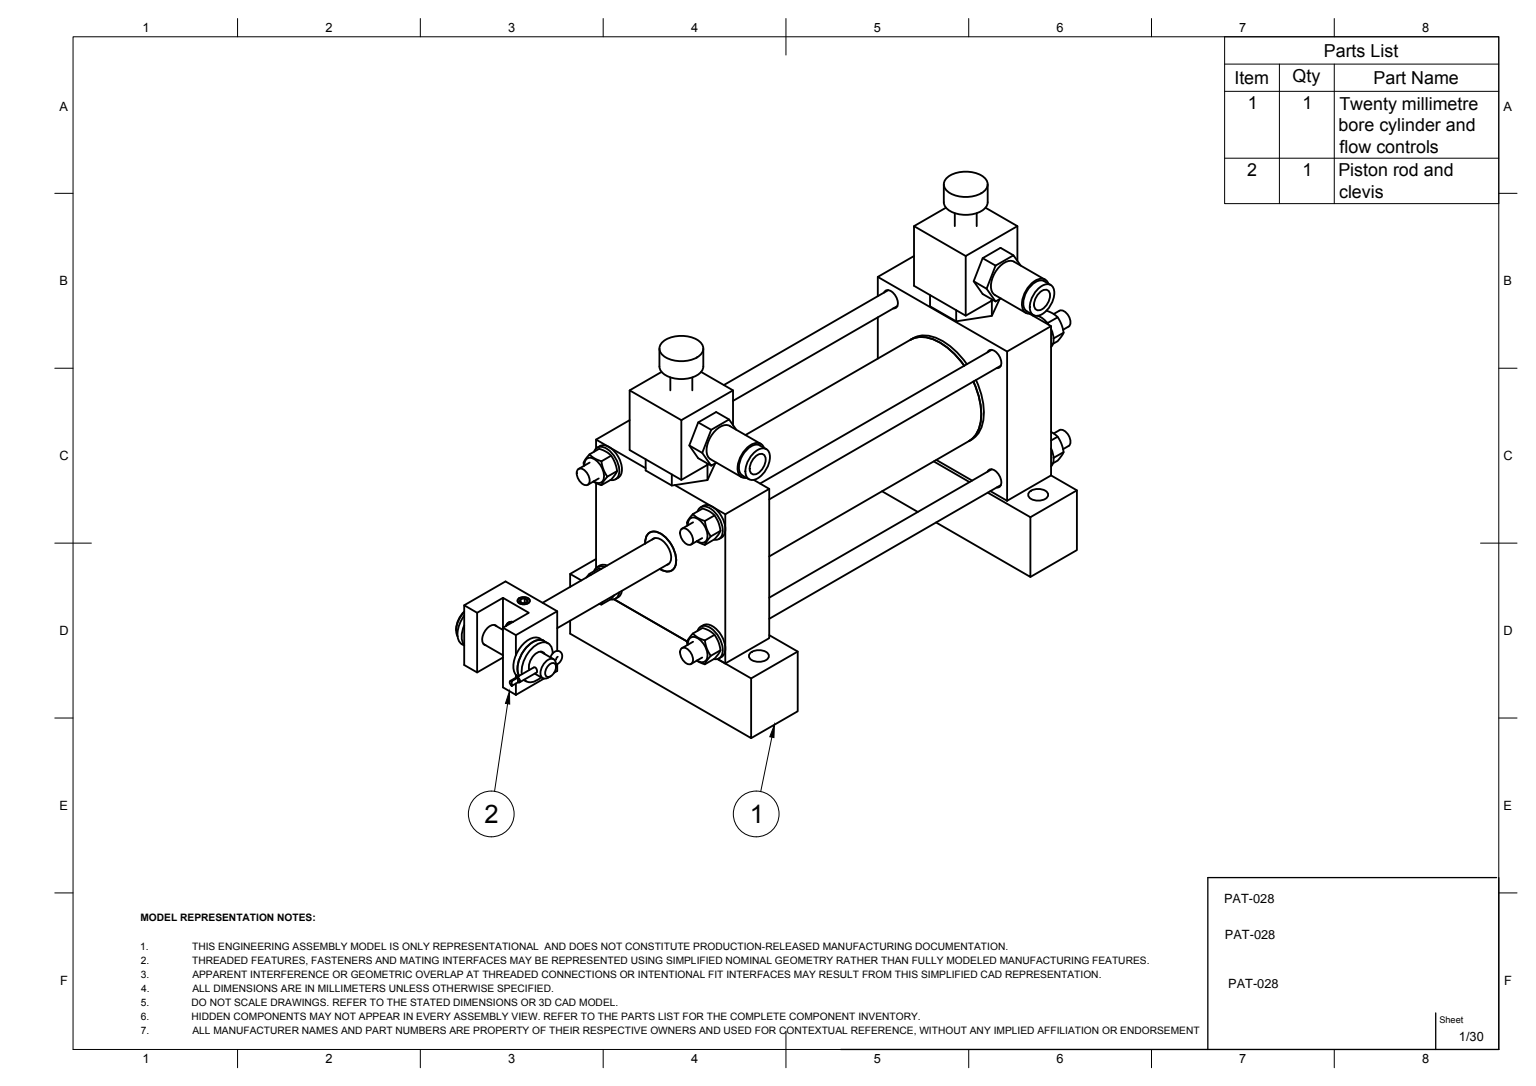
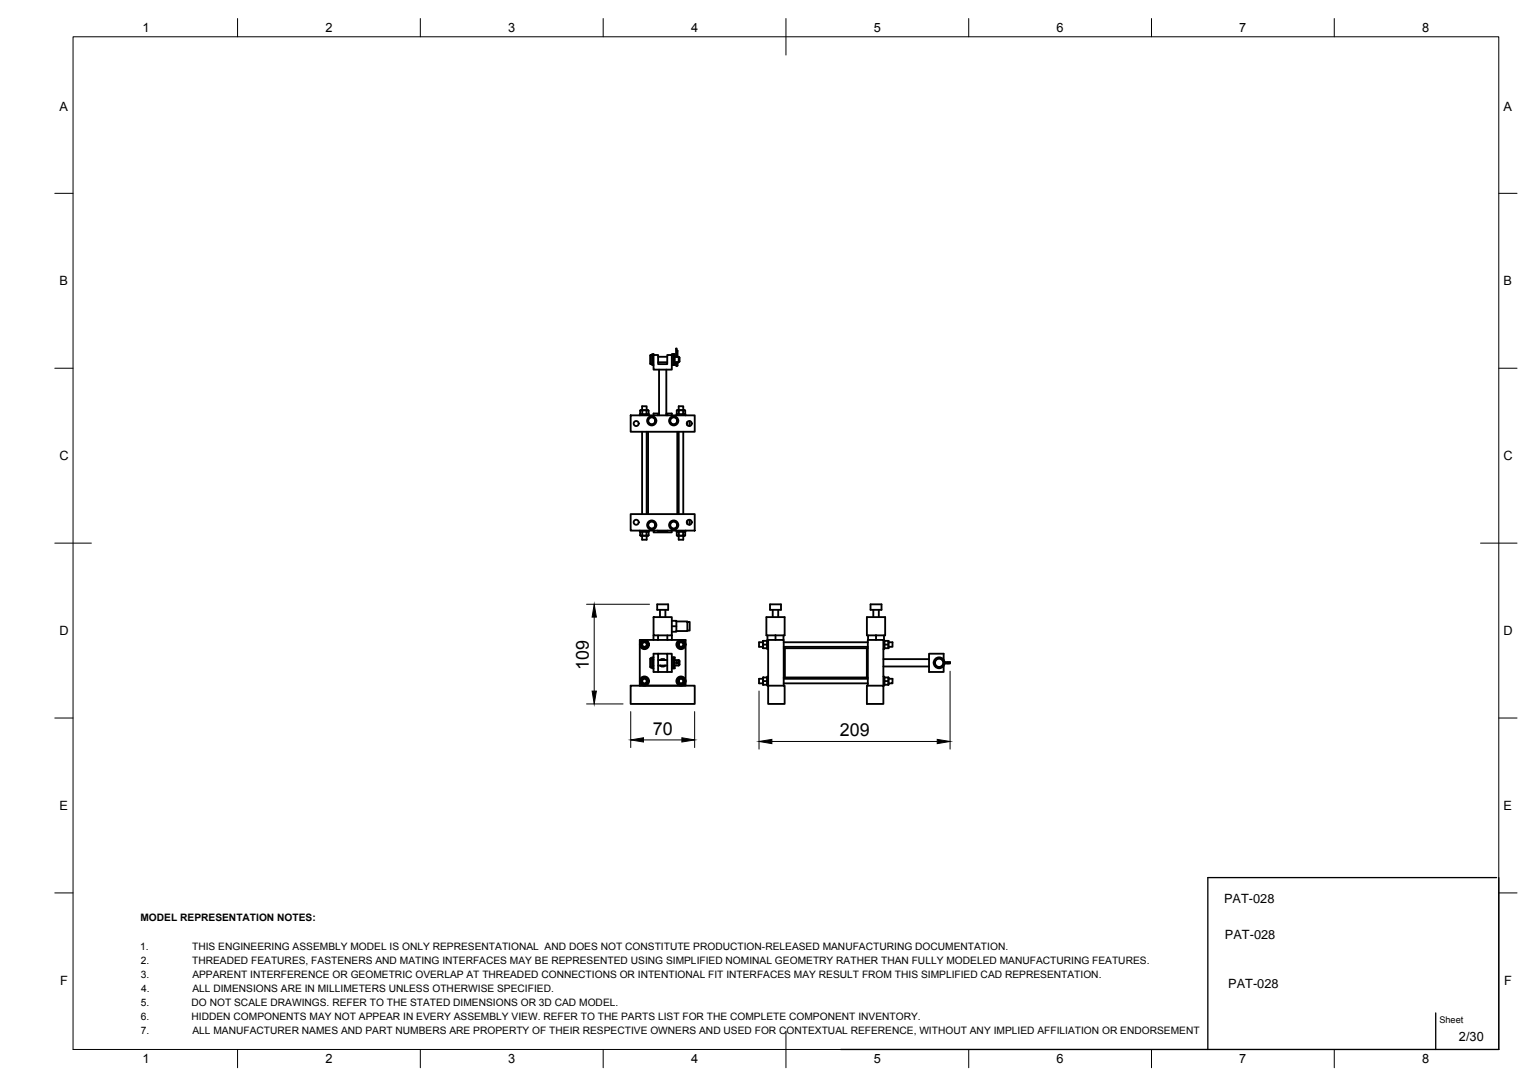
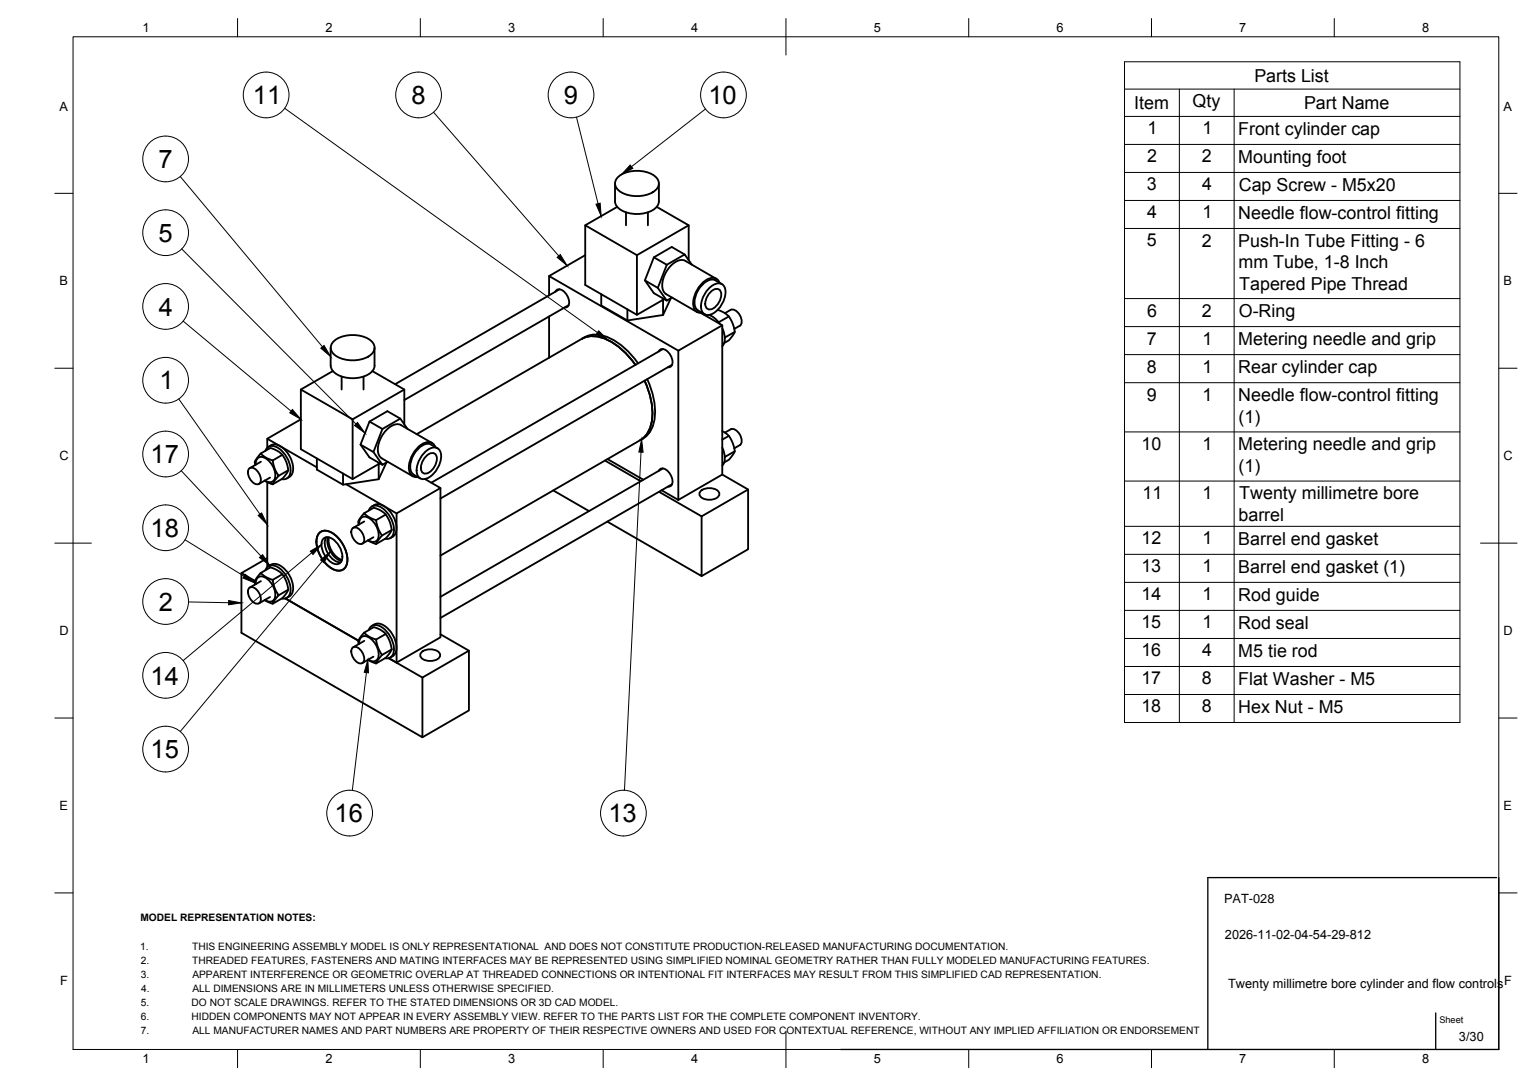
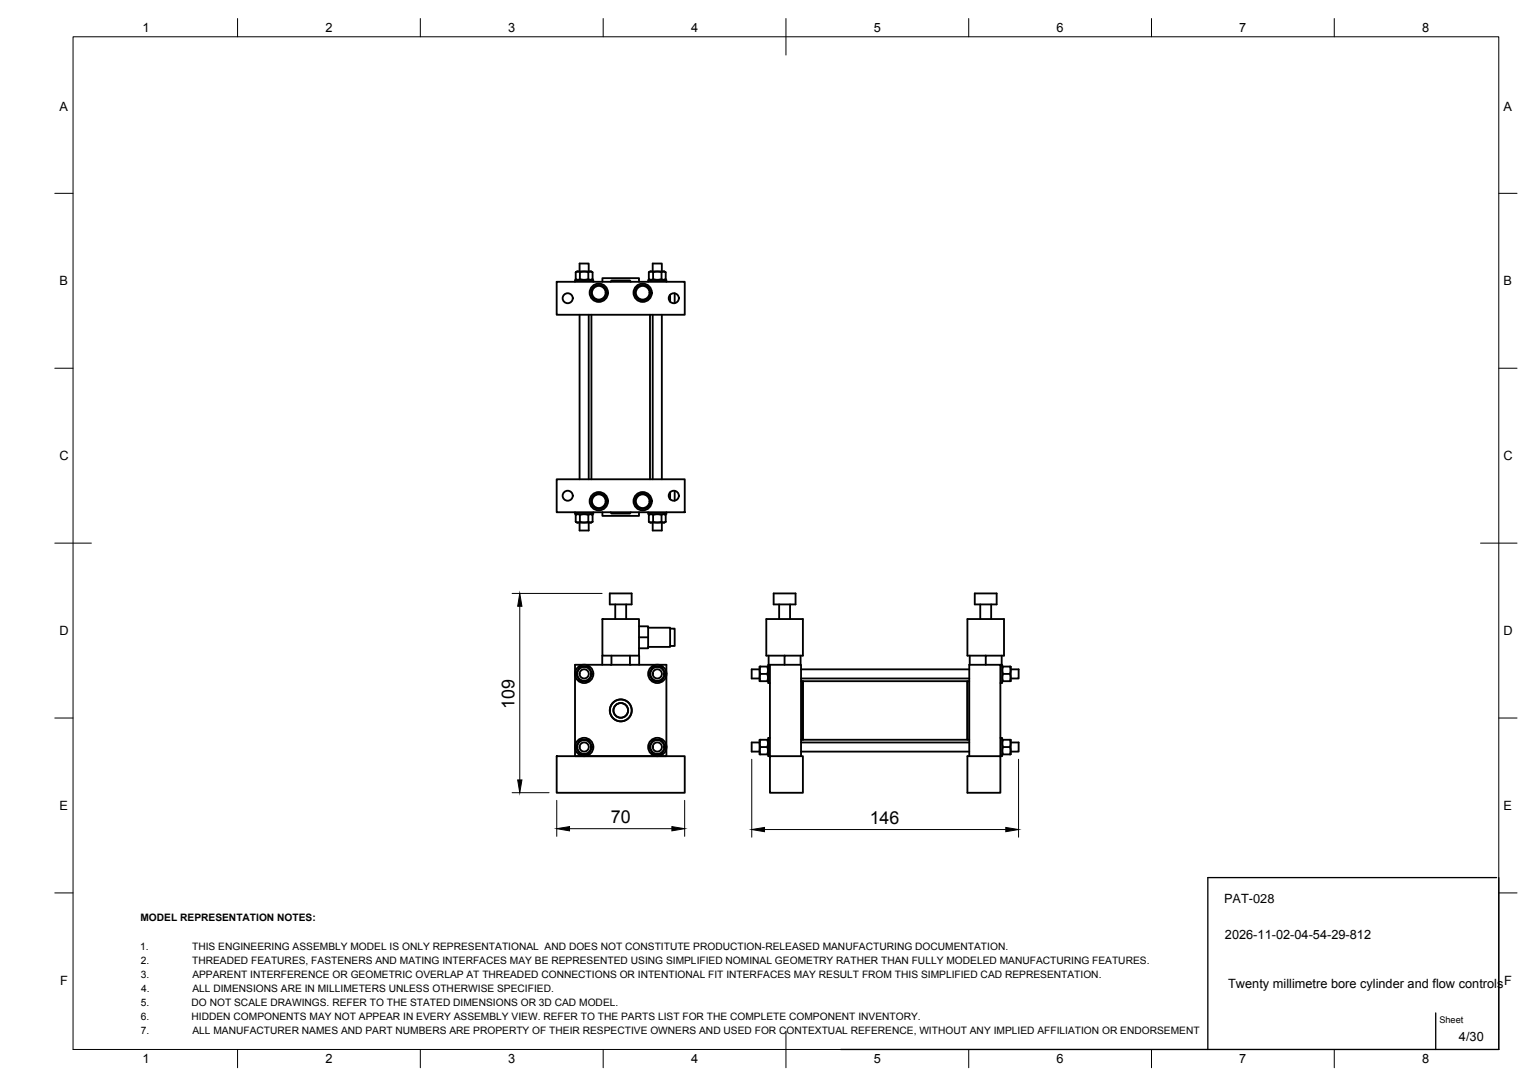
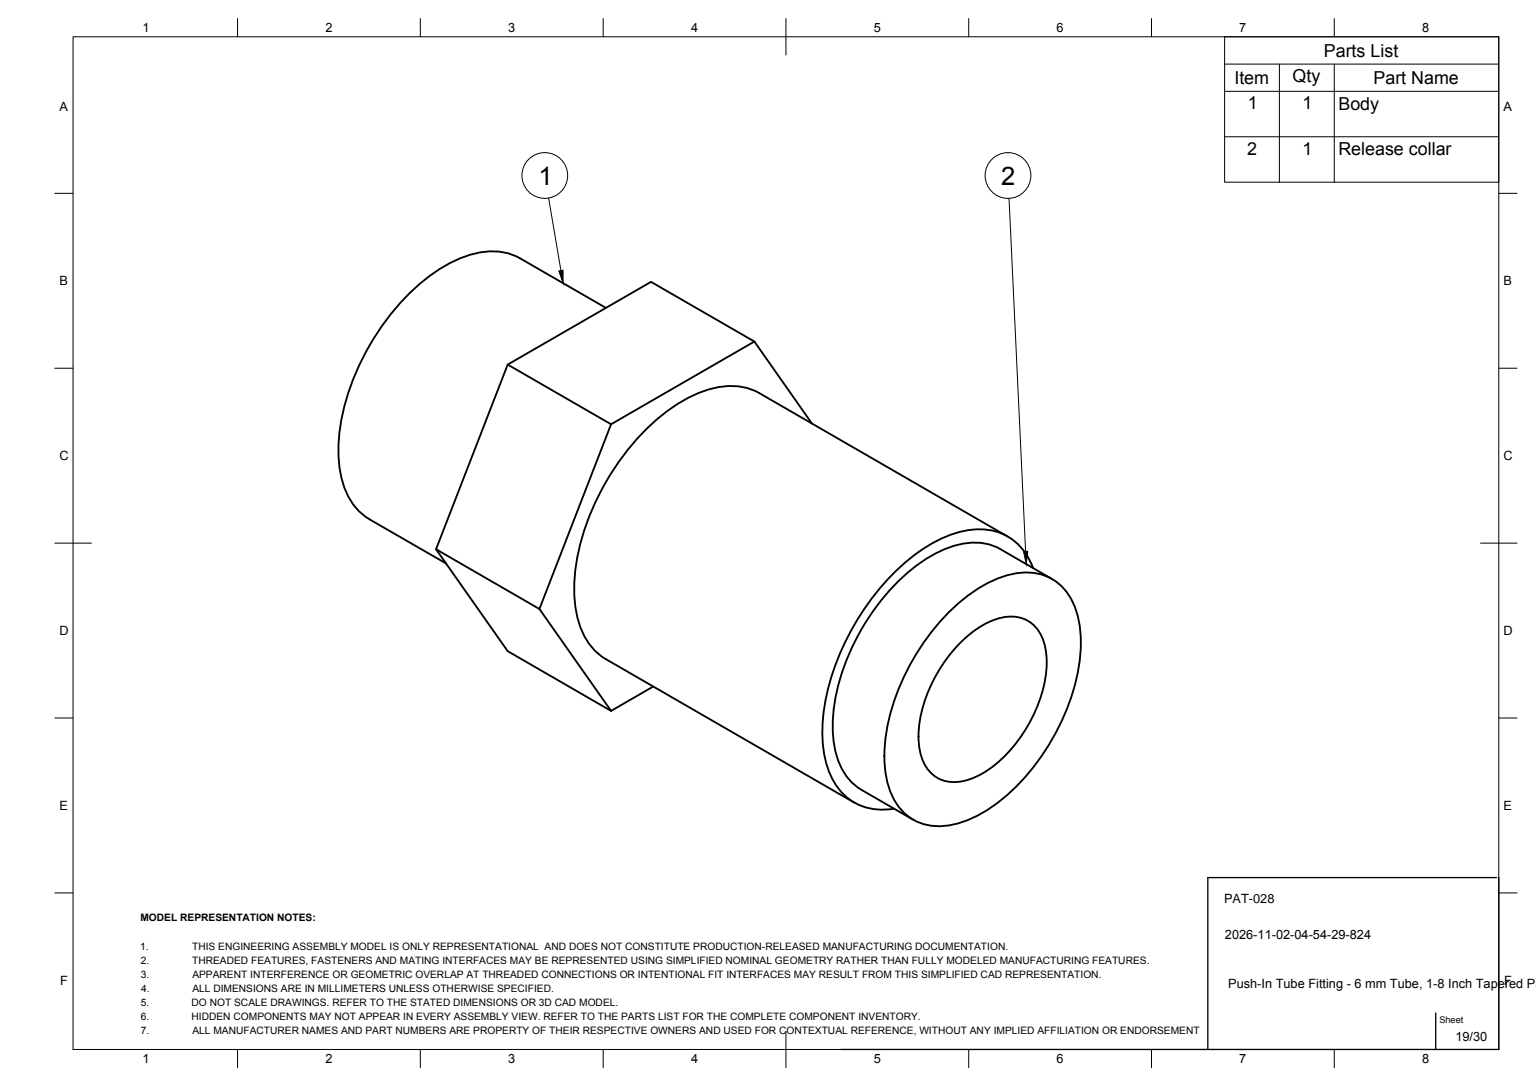
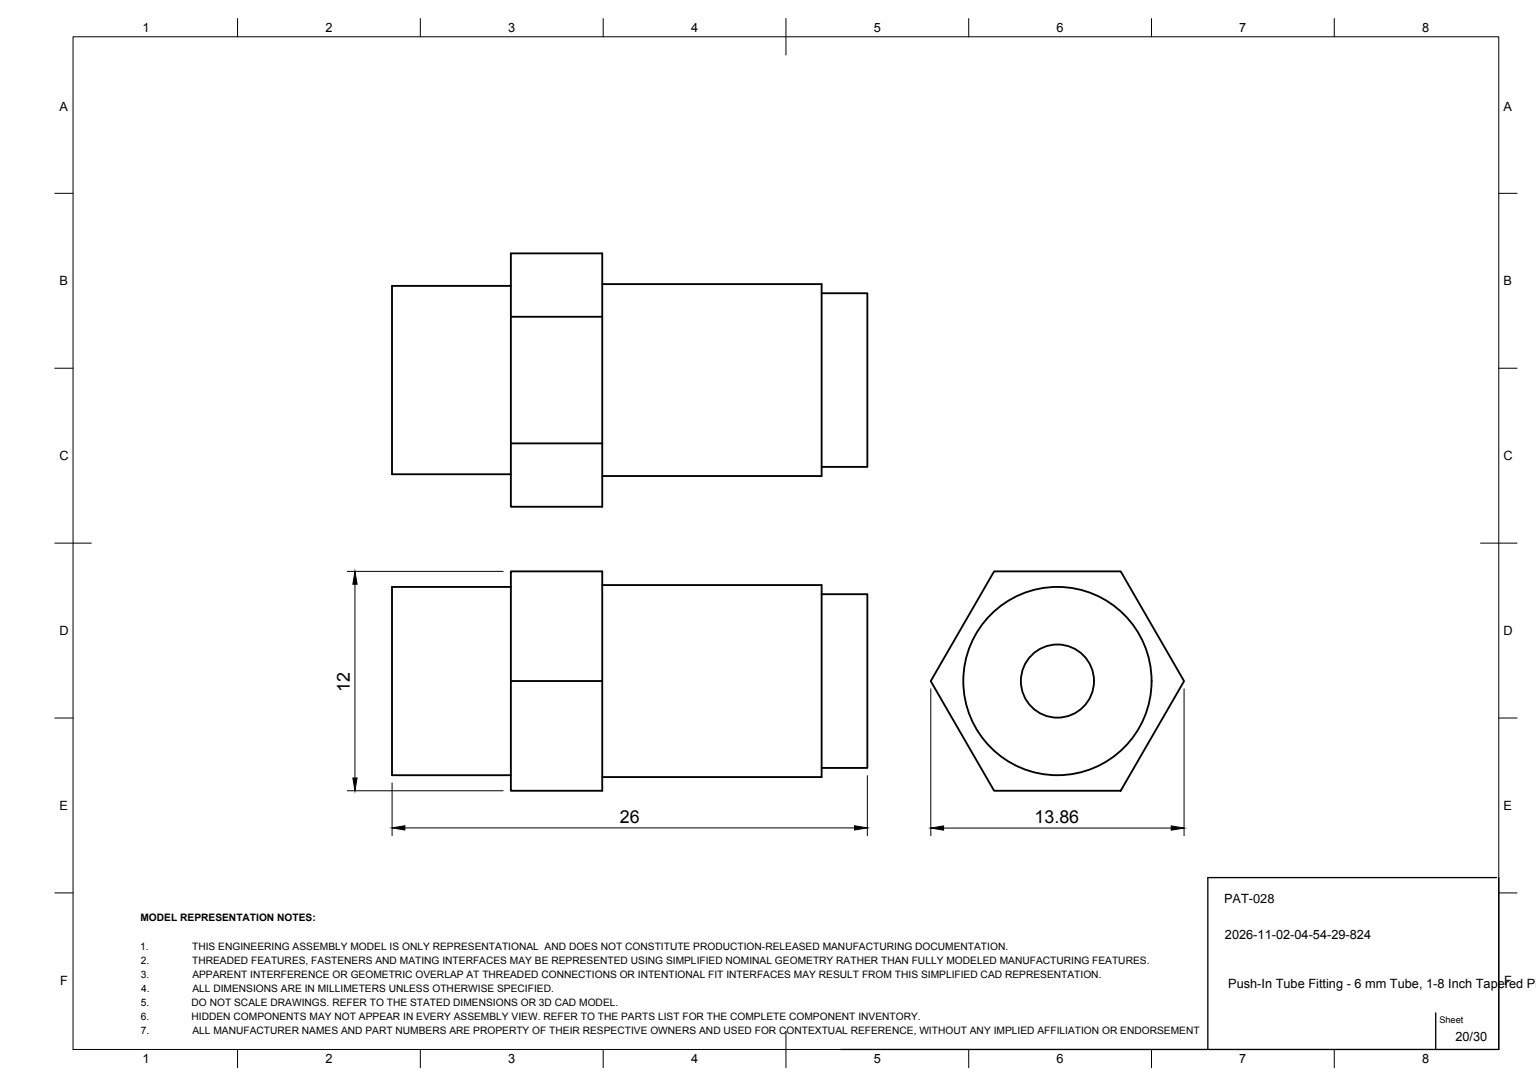
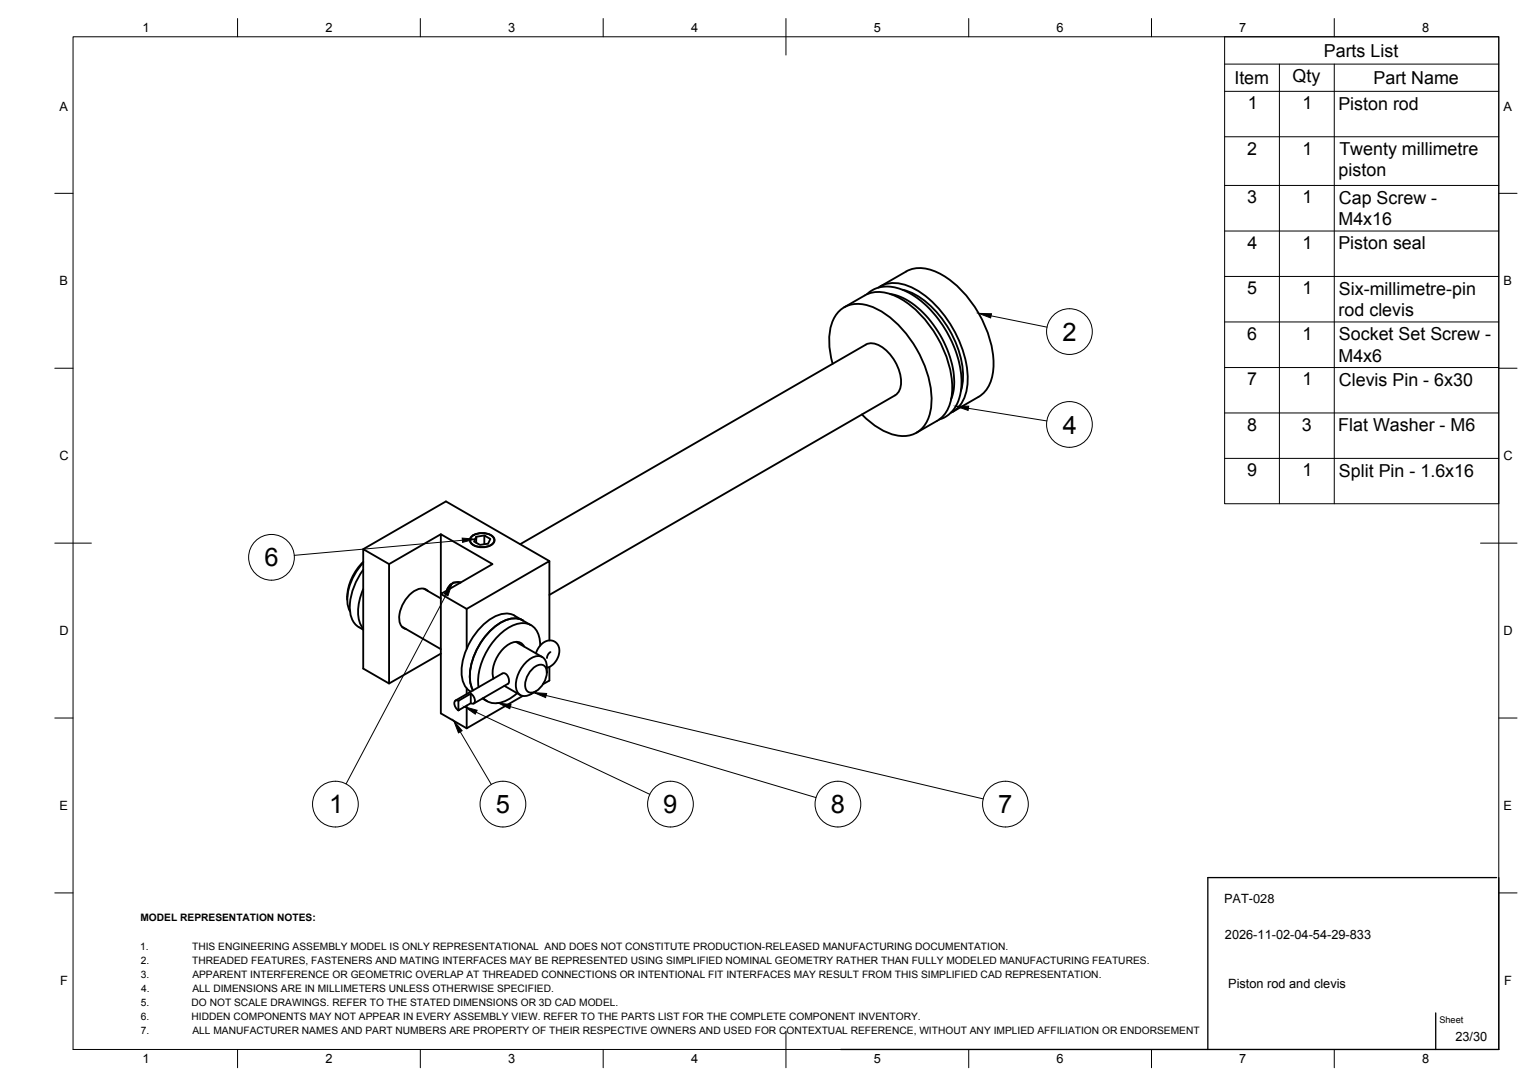
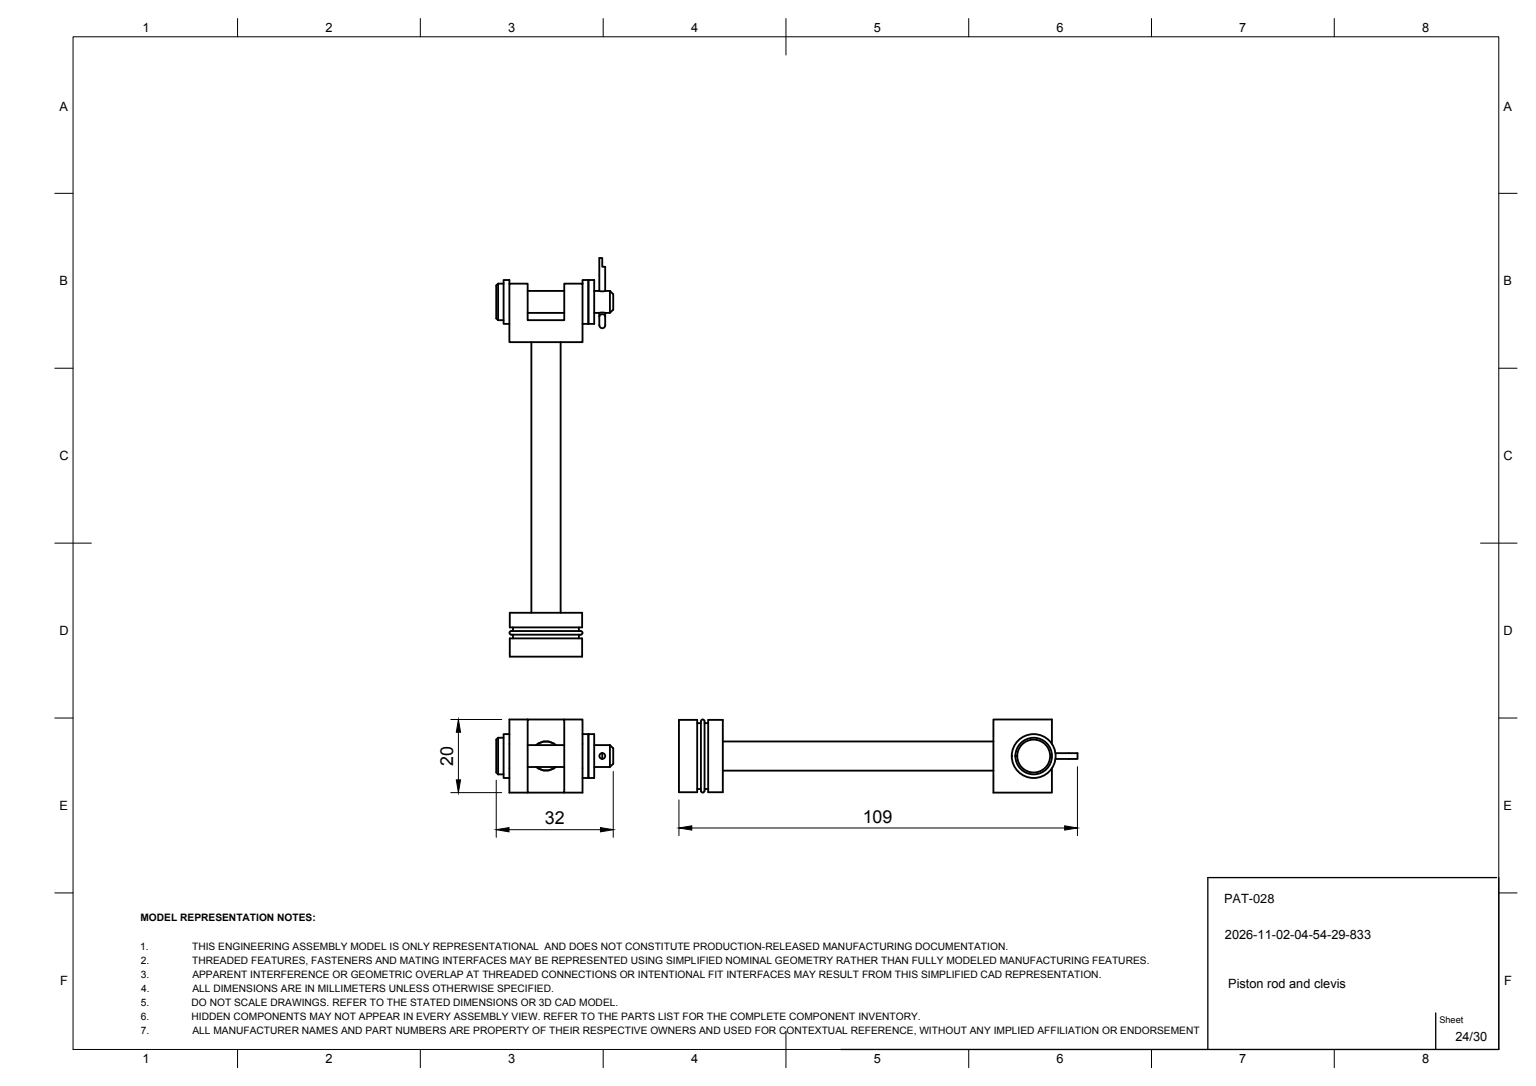
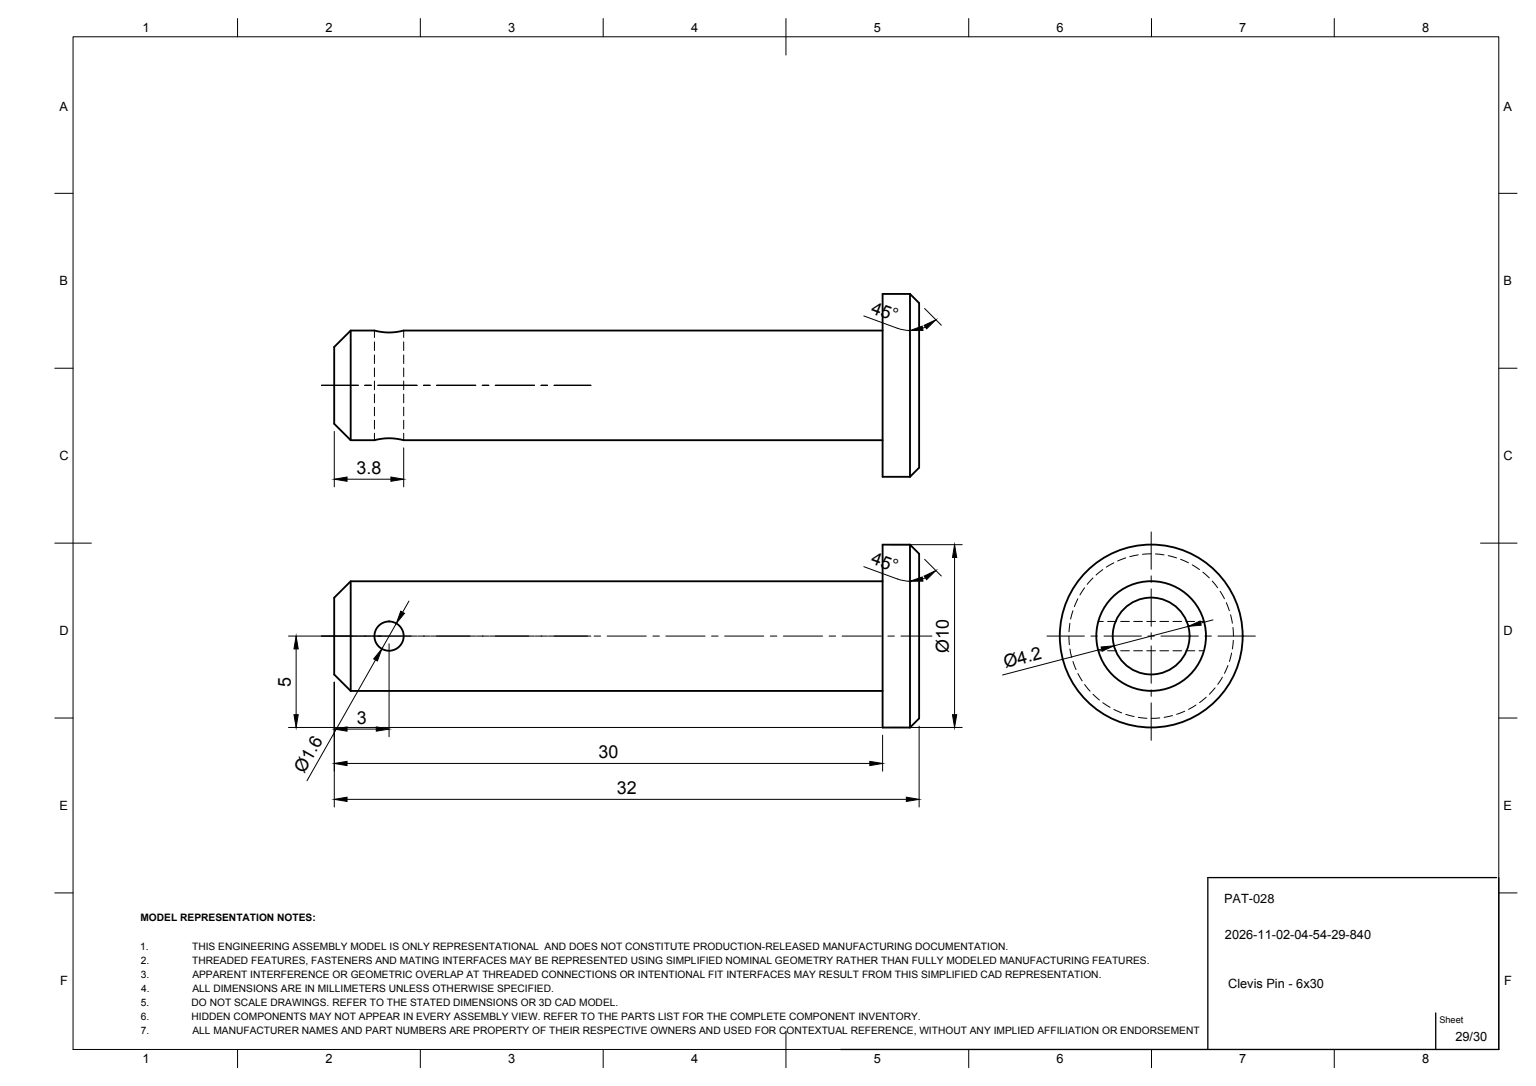
ISO-10303-21;
HEADER;
/* Generated by software containing ST-Developer
 * from STEP Tools, Inc. (www.steptools.com) 
 */

FILE_DESCRIPTION(
/* description */ ('Cylinder foot and clevis mount kit'),
/* implementation_level */ '2;1');

FILE_NAME(
/* name */ 'PAT-028',
/* time_stamp */ '2026-10-27T20:10:43-07:00',
/* author */ (''),
/* organization */ (''),
/* preprocessor_version */ 'ST-DEVELOPER v20.2',
/* originating_system */ 'Autodesk Translation Framework v15.17.0.0',
/* authorisation */ '');

FILE_SCHEMA (('AUTOMOTIVE_DESIGN { 1 0 10303 214 3 1 1 }'));
ENDSEC;

DATA;
#10=MECHANICAL_DESIGN_GEOMETRIC_PRESENTATION_REPRESENTATION('',(#338,#339,
#340,#341,#342,#343,#344,#345,#346,#347,#348,#349,#350,#351,#352,#353,#354,
#355,#356,#357,#358,#359,#360,#361,#362,#363,#364,#365),#9102);
#11=B_SPLINE_CURVE_WITH_KNOTS('',3,(#8691,#8692,#8693,#8694,#8695,#8696,
#8697,#8698,#8699,#8700),.UNSPECIFIED.,.F.,.F.,(4,2,2,2,4),(0.665271585430998,
0.692803751398643,0.75574615888762,0.818688566376597,0.846220732344242),
 .UNSPECIFIED.);
#12=B_SPLINE_CURVE_WITH_KNOTS('',3,(#8708,#8709,#8710,#8711,#8712,#8713,
#8714,#8715,#8716,#8717),.UNSPECIFIED.,.F.,.F.,(4,2,2,2,4),(0.161440812839251,
0.188972978806896,0.251915386295873,0.31485779378485,0.342389959752495),
 .UNSPECIFIED.);
#13=B_SPLINE_CURVE_WITH_KNOTS('',3,(#8834,#8835,#8836,#8837,#8838,#8839,
#8840,#8841,#8842,#8843),.UNSPECIFIED.,.F.,.F.,(4,2,2,2,4),(0.,0.0302963256060356,
0.0605926512120712,0.090883446720838,0.121174242229605),.UNSPECIFIED.);
#14=B_SPLINE_CURVE_WITH_KNOTS('',3,(#8846,#8847,#8848,#8849,#8850,#8851,
#8852,#8853,#8854,#8855,#8856,#8857,#8858,#8859,#8860,#8861,#8862,#8863,
#8864,#8865,#8866,#8867,#8868,#8869,#8870,#8871,#8872,#8873,#8874,#8875,
#8876,#8877,#8878,#8879),.UNSPECIFIED.,.T.,.F.,(4,2,2,2,2,2,2,2,2,2,2,2,
2,2,2,2,4),(0.,0.0302963256060358,0.0605926512120716,0.0908834467208383,
0.121174242229605,0.151465037738372,0.181755833247138,0.212052158853174,
0.24234848445921,0.272644810065246,0.302941135671282,0.333231931180048,
0.363522726688815,0.393813522197582,0.424104317706349,0.454400643312384,
0.48469696891842),.UNSPECIFIED.);
#15=B_SPLINE_CURVE_WITH_KNOTS('',3,(#8881,#8882,#8883,#8884,#8885,#8886,
#8887,#8888,#8889,#8890),.UNSPECIFIED.,.F.,.F.,(4,2,2,2,4),(0.363522726688815,
0.393813522197581,0.424104317706348,0.454400643312384,0.48469696891842),
 .UNSPECIFIED.);
#16=B_SPLINE_CURVE_WITH_KNOTS('',3,(#8891,#8892,#8893,#8894,#8895,#8896,
#8897,#8898,#8899,#8900,#8901,#8902,#8903,#8904,#8905,#8906,#8907,#8908),
 .UNSPECIFIED.,.F.,.F.,(4,2,2,2,2,2,2,2,4),(0.121174242229605,0.151465037738371,
0.181755833247138,0.212052158853174,0.24234848445921,0.272644810065246,
0.302941135671281,0.333231931180048,0.363522726688815),.UNSPECIFIED.);
#17=B_SPLINE_CURVE_WITH_KNOTS('',3,(#8955,#8956,#8957,#8958,#8959,#8960,
#8961,#8962,#8963,#8964,#8965,#8966,#8967,#8968,#8969,#8970,#8971,#8972,
#8973,#8974,#8975,#8976,#8977,#8978,#8979,#8980),.UNSPECIFIED.,.F.,.F.,
(4,2,2,2,2,2,2,2,2,2,2,2,4),(-0.00054581412719389,0.,0.0281583564005144,
0.0618496465371181,0.0905865724114538,0.120694112793616,0.144966158459363,
0.16923820412511,0.199345744507272,0.228082670381608,0.261773960518212,
0.289932316918681,0.290478131045882),.UNSPECIFIED.);
#18=B_SPLINE_CURVE_WITH_KNOTS('',3,(#8981,#8982,#8983,#8984,#8985,#8986,
#8987,#8988,#8989,#8990,#8991,#8992,#8993,#8994,#8995,#8996,#8997,#8998,
#8999,#9000,#9001,#9002,#9003,#9004,#9005,#9006),.UNSPECIFIED.,.F.,.F.,
(4,2,2,2,2,2,2,2,2,2,2,2,4),(-0.000545814127196571,0.,0.0281583564006391,
0.0618496465374156,0.0905865724118984,0.120694112794215,0.144966158460086,
0.169238204125958,0.199345744508275,0.228082670382758,0.261773960519534,
0.289932316920171,0.29047813104737),.UNSPECIFIED.);
#19=(
BOUNDED_CURVE()
B_SPLINE_CURVE(2,(#8429,#8430,#8431),.UNSPECIFIED.,.F.,.F.)
B_SPLINE_CURVE_WITH_KNOTS((3,3),(0.140651836354967,0.670383167684795),
 .UNSPECIFIED.)
CURVE()
GEOMETRIC_REPRESENTATION_ITEM()
RATIONAL_B_SPLINE_CURVE((1.11602540378444,1.28867513459481,1.11602540378444))
REPRESENTATION_ITEM('')
);
#20=(
BOUNDED_CURVE()
B_SPLINE_CURVE(2,(#8433,#8434,#8435),.UNSPECIFIED.,.F.,.F.)
B_SPLINE_CURVE_WITH_KNOTS((3,3),(0.140651836354967,0.670383167684795),
 .UNSPECIFIED.)
CURVE()
GEOMETRIC_REPRESENTATION_ITEM()
RATIONAL_B_SPLINE_CURVE((1.11602540378444,1.28867513459481,1.11602540378444))
REPRESENTATION_ITEM('')
);
#21=(
BOUNDED_CURVE()
B_SPLINE_CURVE(2,(#8440,#8441,#8442),.UNSPECIFIED.,.F.,.F.)
B_SPLINE_CURVE_WITH_KNOTS((3,3),(0.140651836354967,0.670383167684795),
 .UNSPECIFIED.)
CURVE()
GEOMETRIC_REPRESENTATION_ITEM()
RATIONAL_B_SPLINE_CURVE((1.11602540378444,1.28867513459481,1.11602540378444))
REPRESENTATION_ITEM('')
);
#22=(
BOUNDED_CURVE()
B_SPLINE_CURVE(2,(#8444,#8445,#8446),.UNSPECIFIED.,.F.,.F.)
B_SPLINE_CURVE_WITH_KNOTS((3,3),(0.140651836354967,0.670383167684795),
 .UNSPECIFIED.)
CURVE()
GEOMETRIC_REPRESENTATION_ITEM()
RATIONAL_B_SPLINE_CURVE((1.11602540378444,1.28867513459481,1.11602540378444))
REPRESENTATION_ITEM('')
);
#23=(
BOUNDED_CURVE()
B_SPLINE_CURVE(2,(#8448,#8449,#8450),.UNSPECIFIED.,.F.,.F.)
B_SPLINE_CURVE_WITH_KNOTS((3,3),(0.140651836354967,0.670383167684795),
 .UNSPECIFIED.)
CURVE()
GEOMETRIC_REPRESENTATION_ITEM()
RATIONAL_B_SPLINE_CURVE((1.11602540378444,1.28867513459481,1.11602540378444))
REPRESENTATION_ITEM('')
);
#24=(
BOUNDED_CURVE()
B_SPLINE_CURVE(2,(#8451,#8452,#8453),.UNSPECIFIED.,.F.,.F.)
B_SPLINE_CURVE_WITH_KNOTS((3,3),(0.140651836354967,0.670383167684795),
 .UNSPECIFIED.)
CURVE()
GEOMETRIC_REPRESENTATION_ITEM()
RATIONAL_B_SPLINE_CURVE((1.11602540378444,1.28867513459481,1.11602540378444))
REPRESENTATION_ITEM('')
);
#25=(
BOUNDED_CURVE()
B_SPLINE_CURVE(2,(#8460,#8461,#8462),.UNSPECIFIED.,.F.,.F.)
B_SPLINE_CURVE_WITH_KNOTS((3,3),(0.140651836354967,0.670383167684795),
 .UNSPECIFIED.)
CURVE()
GEOMETRIC_REPRESENTATION_ITEM()
RATIONAL_B_SPLINE_CURVE((1.11602540378444,1.28867513459481,1.11602540378444))
REPRESENTATION_ITEM('')
);
#26=(
BOUNDED_CURVE()
B_SPLINE_CURVE(2,(#8464,#8465,#8466),.UNSPECIFIED.,.F.,.F.)
B_SPLINE_CURVE_WITH_KNOTS((3,3),(0.140651836354967,0.670383167684796),
 .UNSPECIFIED.)
CURVE()
GEOMETRIC_REPRESENTATION_ITEM()
RATIONAL_B_SPLINE_CURVE((1.11602540378444,1.28867513459481,1.11602540378444))
REPRESENTATION_ITEM('')
);
#27=(
BOUNDED_CURVE()
B_SPLINE_CURVE(2,(#8468,#8469,#8470),.UNSPECIFIED.,.F.,.F.)
B_SPLINE_CURVE_WITH_KNOTS((3,3),(0.140651836354967,0.670383167684795),
 .UNSPECIFIED.)
CURVE()
GEOMETRIC_REPRESENTATION_ITEM()
RATIONAL_B_SPLINE_CURVE((1.11602540378444,1.28867513459481,1.11602540378444))
REPRESENTATION_ITEM('')
);
#28=(
BOUNDED_CURVE()
B_SPLINE_CURVE(2,(#8472,#8473,#8474),.UNSPECIFIED.,.F.,.F.)
B_SPLINE_CURVE_WITH_KNOTS((3,3),(0.140651836354967,0.670383167684795),
 .UNSPECIFIED.)
CURVE()
GEOMETRIC_REPRESENTATION_ITEM()
RATIONAL_B_SPLINE_CURVE((1.11602540378444,1.28867513459482,1.11602540378444))
REPRESENTATION_ITEM('')
);
#29=(
BOUNDED_CURVE()
B_SPLINE_CURVE(2,(#8476,#8477,#8478),.UNSPECIFIED.,.F.,.F.)
B_SPLINE_CURVE_WITH_KNOTS((3,3),(0.140651836354967,0.670383167684795),
 .UNSPECIFIED.)
CURVE()
GEOMETRIC_REPRESENTATION_ITEM()
RATIONAL_B_SPLINE_CURVE((1.11602540378444,1.28867513459481,1.11602540378444))
REPRESENTATION_ITEM('')
);
#30=(
BOUNDED_CURVE()
B_SPLINE_CURVE(2,(#8479,#8480,#8481),.UNSPECIFIED.,.F.,.F.)
B_SPLINE_CURVE_WITH_KNOTS((3,3),(0.140651836354967,0.670383167684795),
 .UNSPECIFIED.)
CURVE()
GEOMETRIC_REPRESENTATION_ITEM()
RATIONAL_B_SPLINE_CURVE((1.11602540378444,1.28867513459481,1.11602540378444))
REPRESENTATION_ITEM('')
);
#31=TOROIDAL_SURFACE('',#5639,0.3925,0.089);
#32=TOROIDAL_SURFACE('',#5660,0.45,0.05);
#33=TOROIDAL_SURFACE('',#5760,0.95,0.05);
#34=TOROIDAL_SURFACE('',#5868,0.12,0.08);
#35=ITEM_DEFINED_TRANSFORMATION($,$,#5595,#5636);
#36=ITEM_DEFINED_TRANSFORMATION($,$,#5623,#5637);
#37=ITEM_DEFINED_TRANSFORMATION($,$,#5265,#5696);
#38=ITEM_DEFINED_TRANSFORMATION($,$,#5335,#5697);
#39=ITEM_DEFINED_TRANSFORMATION($,$,#5379,#5698);
#40=ITEM_DEFINED_TRANSFORMATION($,$,#5391,#5699);
#41=ITEM_DEFINED_TRANSFORMATION($,$,#5458,#5700);
#42=ITEM_DEFINED_TRANSFORMATION($,$,#5502,#5701);
#43=ITEM_DEFINED_TRANSFORMATION($,$,#5514,#5702);
#44=ITEM_DEFINED_TRANSFORMATION($,$,#5523,#5703);
#45=ITEM_DEFINED_TRANSFORMATION($,$,#5532,#5704);
#46=ITEM_DEFINED_TRANSFORMATION($,$,#5541,#5705);
#47=ITEM_DEFINED_TRANSFORMATION($,$,#5568,#5706);
#48=ITEM_DEFINED_TRANSFORMATION($,$,#5568,#5707);
#49=ITEM_DEFINED_TRANSFORMATION($,$,#5594,#5708);
#50=ITEM_DEFINED_TRANSFORMATION($,$,#5638,#5709);
#51=ITEM_DEFINED_TRANSFORMATION($,$,#5541,#5710);
#52=ITEM_DEFINED_TRANSFORMATION($,$,#5568,#5711);
#53=ITEM_DEFINED_TRANSFORMATION($,$,#5568,#5712);
#54=ITEM_DEFINED_TRANSFORMATION($,$,#5594,#5713);
#55=ITEM_DEFINED_TRANSFORMATION($,$,#5638,#5714);
#56=ITEM_DEFINED_TRANSFORMATION($,$,#5642,#5715);
#57=ITEM_DEFINED_TRANSFORMATION($,$,#5659,#5716);
#58=ITEM_DEFINED_TRANSFORMATION($,$,#5663,#5717);
#59=ITEM_DEFINED_TRANSFORMATION($,$,#5669,#5718);
#60=ITEM_DEFINED_TRANSFORMATION($,$,#5680,#5719);
#61=ITEM_DEFINED_TRANSFORMATION($,$,#5669,#5720);
#62=ITEM_DEFINED_TRANSFORMATION($,$,#5680,#5721);
#63=ITEM_DEFINED_TRANSFORMATION($,$,#5663,#5722);
#64=ITEM_DEFINED_TRANSFORMATION($,$,#5669,#5723);
#65=ITEM_DEFINED_TRANSFORMATION($,$,#5680,#5724);
#66=ITEM_DEFINED_TRANSFORMATION($,$,#5669,#5725);
#67=ITEM_DEFINED_TRANSFORMATION($,$,#5680,#5726);
#68=ITEM_DEFINED_TRANSFORMATION($,$,#5663,#5727);
#69=ITEM_DEFINED_TRANSFORMATION($,$,#5669,#5728);
#70=ITEM_DEFINED_TRANSFORMATION($,$,#5680,#5729);
#71=ITEM_DEFINED_TRANSFORMATION($,$,#5669,#5730);
#72=ITEM_DEFINED_TRANSFORMATION($,$,#5680,#5731);
#73=ITEM_DEFINED_TRANSFORMATION($,$,#5663,#5732);
#74=ITEM_DEFINED_TRANSFORMATION($,$,#5669,#5733);
#75=ITEM_DEFINED_TRANSFORMATION($,$,#5680,#5734);
#76=ITEM_DEFINED_TRANSFORMATION($,$,#5669,#5735);
#77=ITEM_DEFINED_TRANSFORMATION($,$,#5680,#5736);
#78=ITEM_DEFINED_TRANSFORMATION($,$,#5738,#5878);
#79=ITEM_DEFINED_TRANSFORMATION($,$,#5759,#5879);
#80=ITEM_DEFINED_TRANSFORMATION($,$,#5763,#5880);
#81=ITEM_DEFINED_TRANSFORMATION($,$,#5773,#5881);
#82=ITEM_DEFINED_TRANSFORMATION($,$,#5799,#5882);
#83=ITEM_DEFINED_TRANSFORMATION($,$,#5826,#5883);
#84=ITEM_DEFINED_TRANSFORMATION($,$,#5843,#5884);
#85=ITEM_DEFINED_TRANSFORMATION($,$,#5858,#5885);
#86=ITEM_DEFINED_TRANSFORMATION($,$,#5858,#5886);
#87=ITEM_DEFINED_TRANSFORMATION($,$,#5858,#5887);
#88=ITEM_DEFINED_TRANSFORMATION($,$,#5867,#5888);
#89=ITEM_DEFINED_TRANSFORMATION($,$,#5264,#5889);
#90=ITEM_DEFINED_TRANSFORMATION($,$,#5737,#5890);
#91=(
REPRESENTATION_RELATIONSHIP($,$,#9241,#9240)
REPRESENTATION_RELATIONSHIP_WITH_TRANSFORMATION(#35)
SHAPE_REPRESENTATION_RELATIONSHIP()
);
#92=(
REPRESENTATION_RELATIONSHIP($,$,#9242,#9240)
REPRESENTATION_RELATIONSHIP_WITH_TRANSFORMATION(#36)
SHAPE_REPRESENTATION_RELATIONSHIP()
);
#93=(
REPRESENTATION_RELATIONSHIP($,$,#9229,#9228)
REPRESENTATION_RELATIONSHIP_WITH_TRANSFORMATION(#37)
SHAPE_REPRESENTATION_RELATIONSHIP()
);
#94=(
REPRESENTATION_RELATIONSHIP($,$,#9230,#9228)
REPRESENTATION_RELATIONSHIP_WITH_TRANSFORMATION(#38)
SHAPE_REPRESENTATION_RELATIONSHIP()
);
#95=(
REPRESENTATION_RELATIONSHIP($,$,#9231,#9228)
REPRESENTATION_RELATIONSHIP_WITH_TRANSFORMATION(#39)
SHAPE_REPRESENTATION_RELATIONSHIP()
);
#96=(
REPRESENTATION_RELATIONSHIP($,$,#9232,#9228)
REPRESENTATION_RELATIONSHIP_WITH_TRANSFORMATION(#40)
SHAPE_REPRESENTATION_RELATIONSHIP()
);
#97=(
REPRESENTATION_RELATIONSHIP($,$,#9233,#9228)
REPRESENTATION_RELATIONSHIP_WITH_TRANSFORMATION(#41)
SHAPE_REPRESENTATION_RELATIONSHIP()
);
#98=(
REPRESENTATION_RELATIONSHIP($,$,#9234,#9228)
REPRESENTATION_RELATIONSHIP_WITH_TRANSFORMATION(#42)
SHAPE_REPRESENTATION_RELATIONSHIP()
);
#99=(
REPRESENTATION_RELATIONSHIP($,$,#9235,#9228)
REPRESENTATION_RELATIONSHIP_WITH_TRANSFORMATION(#43)
SHAPE_REPRESENTATION_RELATIONSHIP()
);
#100=(
REPRESENTATION_RELATIONSHIP($,$,#9236,#9228)
REPRESENTATION_RELATIONSHIP_WITH_TRANSFORMATION(#44)
SHAPE_REPRESENTATION_RELATIONSHIP()
);
#101=(
REPRESENTATION_RELATIONSHIP($,$,#9237,#9228)
REPRESENTATION_RELATIONSHIP_WITH_TRANSFORMATION(#45)
SHAPE_REPRESENTATION_RELATIONSHIP()
);
#102=(
REPRESENTATION_RELATIONSHIP($,$,#9238,#9228)
REPRESENTATION_RELATIONSHIP_WITH_TRANSFORMATION(#46)
SHAPE_REPRESENTATION_RELATIONSHIP()
);
#103=(
REPRESENTATION_RELATIONSHIP($,$,#9239,#9228)
REPRESENTATION_RELATIONSHIP_WITH_TRANSFORMATION(#47)
SHAPE_REPRESENTATION_RELATIONSHIP()
);
#104=(
REPRESENTATION_RELATIONSHIP($,$,#9239,#9228)
REPRESENTATION_RELATIONSHIP_WITH_TRANSFORMATION(#48)
SHAPE_REPRESENTATION_RELATIONSHIP()
);
#105=(
REPRESENTATION_RELATIONSHIP($,$,#9240,#9228)
REPRESENTATION_RELATIONSHIP_WITH_TRANSFORMATION(#49)
SHAPE_REPRESENTATION_RELATIONSHIP()
);
#106=(
REPRESENTATION_RELATIONSHIP($,$,#9243,#9228)
REPRESENTATION_RELATIONSHIP_WITH_TRANSFORMATION(#50)
SHAPE_REPRESENTATION_RELATIONSHIP()
);
#107=(
REPRESENTATION_RELATIONSHIP($,$,#9238,#9228)
REPRESENTATION_RELATIONSHIP_WITH_TRANSFORMATION(#51)
SHAPE_REPRESENTATION_RELATIONSHIP()
);
#108=(
REPRESENTATION_RELATIONSHIP($,$,#9239,#9228)
REPRESENTATION_RELATIONSHIP_WITH_TRANSFORMATION(#52)
SHAPE_REPRESENTATION_RELATIONSHIP()
);
#109=(
REPRESENTATION_RELATIONSHIP($,$,#9239,#9228)
REPRESENTATION_RELATIONSHIP_WITH_TRANSFORMATION(#53)
SHAPE_REPRESENTATION_RELATIONSHIP()
);
#110=(
REPRESENTATION_RELATIONSHIP($,$,#9240,#9228)
REPRESENTATION_RELATIONSHIP_WITH_TRANSFORMATION(#54)
SHAPE_REPRESENTATION_RELATIONSHIP()
);
#111=(
REPRESENTATION_RELATIONSHIP($,$,#9243,#9228)
REPRESENTATION_RELATIONSHIP_WITH_TRANSFORMATION(#55)
SHAPE_REPRESENTATION_RELATIONSHIP()
);
#112=(
REPRESENTATION_RELATIONSHIP($,$,#9244,#9228)
REPRESENTATION_RELATIONSHIP_WITH_TRANSFORMATION(#56)
SHAPE_REPRESENTATION_RELATIONSHIP()
);
#113=(
REPRESENTATION_RELATIONSHIP($,$,#9245,#9228)
REPRESENTATION_RELATIONSHIP_WITH_TRANSFORMATION(#57)
SHAPE_REPRESENTATION_RELATIONSHIP()
);
#114=(
REPRESENTATION_RELATIONSHIP($,$,#9246,#9228)
REPRESENTATION_RELATIONSHIP_WITH_TRANSFORMATION(#58)
SHAPE_REPRESENTATION_RELATIONSHIP()
);
#115=(
REPRESENTATION_RELATIONSHIP($,$,#9247,#9228)
REPRESENTATION_RELATIONSHIP_WITH_TRANSFORMATION(#59)
SHAPE_REPRESENTATION_RELATIONSHIP()
);
#116=(
REPRESENTATION_RELATIONSHIP($,$,#9248,#9228)
REPRESENTATION_RELATIONSHIP_WITH_TRANSFORMATION(#60)
SHAPE_REPRESENTATION_RELATIONSHIP()
);
#117=(
REPRESENTATION_RELATIONSHIP($,$,#9247,#9228)
REPRESENTATION_RELATIONSHIP_WITH_TRANSFORMATION(#61)
SHAPE_REPRESENTATION_RELATIONSHIP()
);
#118=(
REPRESENTATION_RELATIONSHIP($,$,#9248,#9228)
REPRESENTATION_RELATIONSHIP_WITH_TRANSFORMATION(#62)
SHAPE_REPRESENTATION_RELATIONSHIP()
);
#119=(
REPRESENTATION_RELATIONSHIP($,$,#9246,#9228)
REPRESENTATION_RELATIONSHIP_WITH_TRANSFORMATION(#63)
SHAPE_REPRESENTATION_RELATIONSHIP()
);
#120=(
REPRESENTATION_RELATIONSHIP($,$,#9247,#9228)
REPRESENTATION_RELATIONSHIP_WITH_TRANSFORMATION(#64)
SHAPE_REPRESENTATION_RELATIONSHIP()
);
#121=(
REPRESENTATION_RELATIONSHIP($,$,#9248,#9228)
REPRESENTATION_RELATIONSHIP_WITH_TRANSFORMATION(#65)
SHAPE_REPRESENTATION_RELATIONSHIP()
);
#122=(
REPRESENTATION_RELATIONSHIP($,$,#9247,#9228)
REPRESENTATION_RELATIONSHIP_WITH_TRANSFORMATION(#66)
SHAPE_REPRESENTATION_RELATIONSHIP()
);
#123=(
REPRESENTATION_RELATIONSHIP($,$,#9248,#9228)
REPRESENTATION_RELATIONSHIP_WITH_TRANSFORMATION(#67)
SHAPE_REPRESENTATION_RELATIONSHIP()
);
#124=(
REPRESENTATION_RELATIONSHIP($,$,#9246,#9228)
REPRESENTATION_RELATIONSHIP_WITH_TRANSFORMATION(#68)
SHAPE_REPRESENTATION_RELATIONSHIP()
);
#125=(
REPRESENTATION_RELATIONSHIP($,$,#9247,#9228)
REPRESENTATION_RELATIONSHIP_WITH_TRANSFORMATION(#69)
SHAPE_REPRESENTATION_RELATIONSHIP()
);
#126=(
REPRESENTATION_RELATIONSHIP($,$,#9248,#9228)
REPRESENTATION_RELATIONSHIP_WITH_TRANSFORMATION(#70)
SHAPE_REPRESENTATION_RELATIONSHIP()
);
#127=(
REPRESENTATION_RELATIONSHIP($,$,#9247,#9228)
REPRESENTATION_RELATIONSHIP_WITH_TRANSFORMATION(#71)
SHAPE_REPRESENTATION_RELATIONSHIP()
);
#128=(
REPRESENTATION_RELATIONSHIP($,$,#9248,#9228)
REPRESENTATION_RELATIONSHIP_WITH_TRANSFORMATION(#72)
SHAPE_REPRESENTATION_RELATIONSHIP()
);
#129=(
REPRESENTATION_RELATIONSHIP($,$,#9246,#9228)
REPRESENTATION_RELATIONSHIP_WITH_TRANSFORMATION(#73)
SHAPE_REPRESENTATION_RELATIONSHIP()
);
#130=(
REPRESENTATION_RELATIONSHIP($,$,#9247,#9228)
REPRESENTATION_RELATIONSHIP_WITH_TRANSFORMATION(#74)
SHAPE_REPRESENTATION_RELATIONSHIP()
);
#131=(
REPRESENTATION_RELATIONSHIP($,$,#9248,#9228)
REPRESENTATION_RELATIONSHIP_WITH_TRANSFORMATION(#75)
SHAPE_REPRESENTATION_RELATIONSHIP()
);
#132=(
REPRESENTATION_RELATIONSHIP($,$,#9247,#9228)
REPRESENTATION_RELATIONSHIP_WITH_TRANSFORMATION(#76)
SHAPE_REPRESENTATION_RELATIONSHIP()
);
#133=(
REPRESENTATION_RELATIONSHIP($,$,#9248,#9228)
REPRESENTATION_RELATIONSHIP_WITH_TRANSFORMATION(#77)
SHAPE_REPRESENTATION_RELATIONSHIP()
);
#134=(
REPRESENTATION_RELATIONSHIP($,$,#9250,#9249)
REPRESENTATION_RELATIONSHIP_WITH_TRANSFORMATION(#78)
SHAPE_REPRESENTATION_RELATIONSHIP()
);
#135=(
REPRESENTATION_RELATIONSHIP($,$,#9251,#9249)
REPRESENTATION_RELATIONSHIP_WITH_TRANSFORMATION(#79)
SHAPE_REPRESENTATION_RELATIONSHIP()
);
#136=(
REPRESENTATION_RELATIONSHIP($,$,#9252,#9249)
REPRESENTATION_RELATIONSHIP_WITH_TRANSFORMATION(#80)
SHAPE_REPRESENTATION_RELATIONSHIP()
);
#137=(
REPRESENTATION_RELATIONSHIP($,$,#9253,#9249)
REPRESENTATION_RELATIONSHIP_WITH_TRANSFORMATION(#81)
SHAPE_REPRESENTATION_RELATIONSHIP()
);
#138=(
REPRESENTATION_RELATIONSHIP($,$,#9254,#9249)
REPRESENTATION_RELATIONSHIP_WITH_TRANSFORMATION(#82)
SHAPE_REPRESENTATION_RELATIONSHIP()
);
#139=(
REPRESENTATION_RELATIONSHIP($,$,#9255,#9249)
REPRESENTATION_RELATIONSHIP_WITH_TRANSFORMATION(#83)
SHAPE_REPRESENTATION_RELATIONSHIP()
);
#140=(
REPRESENTATION_RELATIONSHIP($,$,#9256,#9249)
REPRESENTATION_RELATIONSHIP_WITH_TRANSFORMATION(#84)
SHAPE_REPRESENTATION_RELATIONSHIP()
);
#141=(
REPRESENTATION_RELATIONSHIP($,$,#9257,#9249)
REPRESENTATION_RELATIONSHIP_WITH_TRANSFORMATION(#85)
SHAPE_REPRESENTATION_RELATIONSHIP()
);
#142=(
REPRESENTATION_RELATIONSHIP($,$,#9257,#9249)
REPRESENTATION_RELATIONSHIP_WITH_TRANSFORMATION(#86)
SHAPE_REPRESENTATION_RELATIONSHIP()
);
#143=(
REPRESENTATION_RELATIONSHIP($,$,#9257,#9249)
REPRESENTATION_RELATIONSHIP_WITH_TRANSFORMATION(#87)
SHAPE_REPRESENTATION_RELATIONSHIP()
);
#144=(
REPRESENTATION_RELATIONSHIP($,$,#9258,#9249)
REPRESENTATION_RELATIONSHIP_WITH_TRANSFORMATION(#88)
SHAPE_REPRESENTATION_RELATIONSHIP()
);
#145=(
REPRESENTATION_RELATIONSHIP($,$,#9228,#9227)
REPRESENTATION_RELATIONSHIP_WITH_TRANSFORMATION(#89)
SHAPE_REPRESENTATION_RELATIONSHIP()
);
#146=(
REPRESENTATION_RELATIONSHIP($,$,#9249,#9227)
REPRESENTATION_RELATIONSHIP_WITH_TRANSFORMATION(#90)
SHAPE_REPRESENTATION_RELATIONSHIP()
);
#147=CONTEXT_DEPENDENT_SHAPE_REPRESENTATION(#91,#9155);
#148=CONTEXT_DEPENDENT_SHAPE_REPRESENTATION(#92,#9156);
#149=CONTEXT_DEPENDENT_SHAPE_REPRESENTATION(#93,#9163);
#150=CONTEXT_DEPENDENT_SHAPE_REPRESENTATION(#94,#9164);
#151=CONTEXT_DEPENDENT_SHAPE_REPRESENTATION(#95,#9165);
#152=CONTEXT_DEPENDENT_SHAPE_REPRESENTATION(#96,#9166);
#153=CONTEXT_DEPENDENT_SHAPE_REPRESENTATION(#97,#9167);
#154=CONTEXT_DEPENDENT_SHAPE_REPRESENTATION(#98,#9168);
#155=CONTEXT_DEPENDENT_SHAPE_REPRESENTATION(#99,#9169);
#156=CONTEXT_DEPENDENT_SHAPE_REPRESENTATION(#100,#9170);
#157=CONTEXT_DEPENDENT_SHAPE_REPRESENTATION(#101,#9171);
#158=CONTEXT_DEPENDENT_SHAPE_REPRESENTATION(#102,#9172);
#159=CONTEXT_DEPENDENT_SHAPE_REPRESENTATION(#103,#9173);
#160=CONTEXT_DEPENDENT_SHAPE_REPRESENTATION(#104,#9174);
#161=CONTEXT_DEPENDENT_SHAPE_REPRESENTATION(#105,#9175);
#162=CONTEXT_DEPENDENT_SHAPE_REPRESENTATION(#106,#9176);
#163=CONTEXT_DEPENDENT_SHAPE_REPRESENTATION(#107,#9177);
#164=CONTEXT_DEPENDENT_SHAPE_REPRESENTATION(#108,#9178);
#165=CONTEXT_DEPENDENT_SHAPE_REPRESENTATION(#109,#9179);
#166=CONTEXT_DEPENDENT_SHAPE_REPRESENTATION(#110,#9180);
#167=CONTEXT_DEPENDENT_SHAPE_REPRESENTATION(#111,#9181);
#168=CONTEXT_DEPENDENT_SHAPE_REPRESENTATION(#112,#9182);
#169=CONTEXT_DEPENDENT_SHAPE_REPRESENTATION(#113,#9183);
#170=CONTEXT_DEPENDENT_SHAPE_REPRESENTATION(#114,#9184);
#171=CONTEXT_DEPENDENT_SHAPE_REPRESENTATION(#115,#9185);
#172=CONTEXT_DEPENDENT_SHAPE_REPRESENTATION(#116,#9186);
#173=CONTEXT_DEPENDENT_SHAPE_REPRESENTATION(#117,#9187);
#174=CONTEXT_DEPENDENT_SHAPE_REPRESENTATION(#118,#9188);
#175=CONTEXT_DEPENDENT_SHAPE_REPRESENTATION(#119,#9189);
#176=CONTEXT_DEPENDENT_SHAPE_REPRESENTATION(#120,#9190);
#177=CONTEXT_DEPENDENT_SHAPE_REPRESENTATION(#121,#9191);
#178=CONTEXT_DEPENDENT_SHAPE_REPRESENTATION(#122,#9192);
#179=CONTEXT_DEPENDENT_SHAPE_REPRESENTATION(#123,#9193);
#180=CONTEXT_DEPENDENT_SHAPE_REPRESENTATION(#124,#9194);
#181=CONTEXT_DEPENDENT_SHAPE_REPRESENTATION(#125,#9195);
#182=CONTEXT_DEPENDENT_SHAPE_REPRESENTATION(#126,#9196);
#183=CONTEXT_DEPENDENT_SHAPE_REPRESENTATION(#127,#9197);
#184=CONTEXT_DEPENDENT_SHAPE_REPRESENTATION(#128,#9198);
#185=CONTEXT_DEPENDENT_SHAPE_REPRESENTATION(#129,#9199);
#186=CONTEXT_DEPENDENT_SHAPE_REPRESENTATION(#130,#9200);
#187=CONTEXT_DEPENDENT_SHAPE_REPRESENTATION(#131,#9201);
#188=CONTEXT_DEPENDENT_SHAPE_REPRESENTATION(#132,#9202);
#189=CONTEXT_DEPENDENT_SHAPE_REPRESENTATION(#133,#9203);
#190=CONTEXT_DEPENDENT_SHAPE_REPRESENTATION(#134,#9214);
#191=CONTEXT_DEPENDENT_SHAPE_REPRESENTATION(#135,#9215);
#192=CONTEXT_DEPENDENT_SHAPE_REPRESENTATION(#136,#9216);
#193=CONTEXT_DEPENDENT_SHAPE_REPRESENTATION(#137,#9217);
#194=CONTEXT_DEPENDENT_SHAPE_REPRESENTATION(#138,#9218);
#195=CONTEXT_DEPENDENT_SHAPE_REPRESENTATION(#139,#9219);
#196=CONTEXT_DEPENDENT_SHAPE_REPRESENTATION(#140,#9220);
#197=CONTEXT_DEPENDENT_SHAPE_REPRESENTATION(#141,#9221);
#198=CONTEXT_DEPENDENT_SHAPE_REPRESENTATION(#142,#9222);
#199=CONTEXT_DEPENDENT_SHAPE_REPRESENTATION(#143,#9223);
#200=CONTEXT_DEPENDENT_SHAPE_REPRESENTATION(#144,#9224);
#201=CONTEXT_DEPENDENT_SHAPE_REPRESENTATION(#145,#9225);
#202=CONTEXT_DEPENDENT_SHAPE_REPRESENTATION(#146,#9226);
#203=NEXT_ASSEMBLY_USAGE_OCCURRENCE('Body:1','Body:1','Body:1',#9273,#9274,
'Body:1');
#204=NEXT_ASSEMBLY_USAGE_OCCURRENCE('Release collar:1',
'Release collar:1','Release collar:1',#9273,#9275,'Release collar:1');
#205=NEXT_ASSEMBLY_USAGE_OCCURRENCE('Front cylinder cap:1',
'Front cylinder cap:1','Front cylinder cap:1',#9261,#9262,
'Front cylinder cap:1');
#206=NEXT_ASSEMBLY_USAGE_OCCURRENCE('Needle flow-control fitting:1',
'Needle flow-control fitting:1','Needle flow-control fitting:1',#9261,#9263,
'Needle flow-control fitting:1');
#207=NEXT_ASSEMBLY_USAGE_OCCURRENCE('Metering needle and grip:1',
'Metering needle and grip:1','Metering needle and grip:1',#9261,#9264,
'Metering needle and grip:1');
#208=NEXT_ASSEMBLY_USAGE_OCCURRENCE('Rear cylinder cap:1',
'Rear cylinder cap:1','Rear cylinder cap:1',#9261,#9265,
'Rear cylinder cap:1');
#209=NEXT_ASSEMBLY_USAGE_OCCURRENCE('Needle flow-control fitting (1):1',
'Needle flow-control fitting (1):1','Needle flow-control fitting (1):1',
#9261,#9266,'Needle flow-control fitting (1):1');
#210=NEXT_ASSEMBLY_USAGE_OCCURRENCE('Metering needle and grip (1):1',
'Metering needle and grip (1):1','Metering needle and grip (1):1',#9261,
#9267,'Metering needle and grip (1):1');
#211=NEXT_ASSEMBLY_USAGE_OCCURRENCE('Twenty millimetre bore barrel:1',
'Twenty millimetre bore barrel:1','Twenty millimetre bore barrel:1',#9261,
#9268,'Twenty millimetre bore barrel:1');
#212=NEXT_ASSEMBLY_USAGE_OCCURRENCE('Barrel end gasket:1',
'Barrel end gasket:1','Barrel end gasket:1',#9261,#9269,
'Barrel end gasket:1');
#213=NEXT_ASSEMBLY_USAGE_OCCURRENCE('Barrel end gasket (1):1',
'Barrel end gasket (1):1','Barrel end gasket (1):1',#9261,#9270,
'Barrel end gasket (1):1');
#214=NEXT_ASSEMBLY_USAGE_OCCURRENCE('Mounting foot:2','Mounting foot:2',
'Mounting foot:2',#9261,#9271,'Mounting foot:2');
#215=NEXT_ASSEMBLY_USAGE_OCCURRENCE('Cap Screw - M5x20:2',
'Cap Screw - M5x20:2','Cap Screw - M5x20:2',#9261,#9272,
'Cap Screw - M5x20:2');
#216=NEXT_ASSEMBLY_USAGE_OCCURRENCE('Cap Screw - M5x20:3',
'Cap Screw - M5x20:3','Cap Screw - M5x20:3',#9261,#9272,
'Cap Screw - M5x20:3');
#217=NEXT_ASSEMBLY_USAGE_OCCURRENCE(
'Push-In Tube Fitting - 6 mm Tube, 1-8 Inch Tapered Pipe Thread:2',
'Push-In Tube Fitting - 6 mm Tube, 1-8 Inch Tapered Pipe Thread:2',
'Push-In Tube Fitting - 6 mm Tube, 1-8 Inch Tapered Pipe Thread:2',#9261,
#9273,
'Push-In Tube Fitting - 6 mm Tube, 1-8 Inch Tapered Pipe Thread:2');
#218=NEXT_ASSEMBLY_USAGE_OCCURRENCE('O-Ring:2','O-Ring:2','O-Ring:2',#9261,
#9276,'O-Ring:2');
#219=NEXT_ASSEMBLY_USAGE_OCCURRENCE('Mounting foot:3','Mounting foot:3',
'Mounting foot:3',#9261,#9271,'Mounting foot:3');
#220=NEXT_ASSEMBLY_USAGE_OCCURRENCE('Cap Screw - M5x20:4',
'Cap Screw - M5x20:4','Cap Screw - M5x20:4',#9261,#9272,
'Cap Screw - M5x20:4');
#221=NEXT_ASSEMBLY_USAGE_OCCURRENCE('Cap Screw - M5x20:5',
'Cap Screw - M5x20:5','Cap Screw - M5x20:5',#9261,#9272,
'Cap Screw - M5x20:5');
#222=NEXT_ASSEMBLY_USAGE_OCCURRENCE(
'Push-In Tube Fitting - 6 mm Tube, 1-8 Inch Tapered Pipe Thread:3',
'Push-In Tube Fitting - 6 mm Tube, 1-8 Inch Tapered Pipe Thread:3',
'Push-In Tube Fitting - 6 mm Tube, 1-8 Inch Tapered Pipe Thread:3',#9261,
#9273,
'Push-In Tube Fitting - 6 mm Tube, 1-8 Inch Tapered Pipe Thread:3');
#223=NEXT_ASSEMBLY_USAGE_OCCURRENCE('O-Ring:3','O-Ring:3','O-Ring:3',#9261,
#9276,'O-Ring:3');
#224=NEXT_ASSEMBLY_USAGE_OCCURRENCE('Rod guide:2','Rod guide:2',
'Rod guide:2',#9261,#9277,'Rod guide:2');
#225=NEXT_ASSEMBLY_USAGE_OCCURRENCE('Rod seal:2','Rod seal:2',
'Rod seal:2',#9261,#9278,'Rod seal:2');
#226=NEXT_ASSEMBLY_USAGE_OCCURRENCE('M5 tie rod:2','M5 tie rod:2',
'M5 tie rod:2',#9261,#9279,'M5 tie rod:2');
#227=NEXT_ASSEMBLY_USAGE_OCCURRENCE('Flat Washer - M5:2',
'Flat Washer - M5:2','Flat Washer - M5:2',#9261,#9280,
'Flat Washer - M5:2');
#228=NEXT_ASSEMBLY_USAGE_OCCURRENCE('Hex Nut - M5:2','Hex Nut - M5:2',
'Hex Nut - M5:2',#9261,#9281,'Hex Nut - M5:2');
#229=NEXT_ASSEMBLY_USAGE_OCCURRENCE('Flat Washer - M5:3',
'Flat Washer - M5:3','Flat Washer - M5:3',#9261,#9280,
'Flat Washer - M5:3');
#230=NEXT_ASSEMBLY_USAGE_OCCURRENCE('Hex Nut - M5:3','Hex Nut - M5:3',
'Hex Nut - M5:3',#9261,#9281,'Hex Nut - M5:3');
#231=NEXT_ASSEMBLY_USAGE_OCCURRENCE('M5 tie rod:3','M5 tie rod:3',
'M5 tie rod:3',#9261,#9279,'M5 tie rod:3');
#232=NEXT_ASSEMBLY_USAGE_OCCURRENCE('Flat Washer - M5:4',
'Flat Washer - M5:4','Flat Washer - M5:4',#9261,#9280,
'Flat Washer - M5:4');
#233=NEXT_ASSEMBLY_USAGE_OCCURRENCE('Hex Nut - M5:4','Hex Nut - M5:4',
'Hex Nut - M5:4',#9261,#9281,'Hex Nut - M5:4');
#234=NEXT_ASSEMBLY_USAGE_OCCURRENCE('Flat Washer - M5:5',
'Flat Washer - M5:5','Flat Washer - M5:5',#9261,#9280,
'Flat Washer - M5:5');
#235=NEXT_ASSEMBLY_USAGE_OCCURRENCE('Hex Nut - M5:5','Hex Nut - M5:5',
'Hex Nut - M5:5',#9261,#9281,'Hex Nut - M5:5');
#236=NEXT_ASSEMBLY_USAGE_OCCURRENCE('M5 tie rod:4','M5 tie rod:4',
'M5 tie rod:4',#9261,#9279,'M5 tie rod:4');
#237=NEXT_ASSEMBLY_USAGE_OCCURRENCE('Flat Washer - M5:6',
'Flat Washer - M5:6','Flat Washer - M5:6',#9261,#9280,
'Flat Washer - M5:6');
#238=NEXT_ASSEMBLY_USAGE_OCCURRENCE('Hex Nut - M5:6','Hex Nut - M5:6',
'Hex Nut - M5:6',#9261,#9281,'Hex Nut - M5:6');
#239=NEXT_ASSEMBLY_USAGE_OCCURRENCE('Flat Washer - M5:7',
'Flat Washer - M5:7','Flat Washer - M5:7',#9261,#9280,
'Flat Washer - M5:7');
#240=NEXT_ASSEMBLY_USAGE_OCCURRENCE('Hex Nut - M5:7','Hex Nut - M5:7',
'Hex Nut - M5:7',#9261,#9281,'Hex Nut - M5:7');
#241=NEXT_ASSEMBLY_USAGE_OCCURRENCE('M5 tie rod:5','M5 tie rod:5',
'M5 tie rod:5',#9261,#9279,'M5 tie rod:5');
#242=NEXT_ASSEMBLY_USAGE_OCCURRENCE('Flat Washer - M5:8',
'Flat Washer - M5:8','Flat Washer - M5:8',#9261,#9280,
'Flat Washer - M5:8');
#243=NEXT_ASSEMBLY_USAGE_OCCURRENCE('Hex Nut - M5:8','Hex Nut - M5:8',
'Hex Nut - M5:8',#9261,#9281,'Hex Nut - M5:8');
#244=NEXT_ASSEMBLY_USAGE_OCCURRENCE('Flat Washer - M5:9',
'Flat Washer - M5:9','Flat Washer - M5:9',#9261,#9280,
'Flat Washer - M5:9');
#245=NEXT_ASSEMBLY_USAGE_OCCURRENCE('Hex Nut - M5:9','Hex Nut - M5:9',
'Hex Nut - M5:9',#9261,#9281,'Hex Nut - M5:9');
#246=NEXT_ASSEMBLY_USAGE_OCCURRENCE('Twenty millimetre piston:1',
'Twenty millimetre piston:1','Twenty millimetre piston:1',#9282,#9283,
'Twenty millimetre piston:1');
#247=NEXT_ASSEMBLY_USAGE_OCCURRENCE('Piston seal:1','Piston seal:1',
'Piston seal:1',#9282,#9284,'Piston seal:1');
#248=NEXT_ASSEMBLY_USAGE_OCCURRENCE('Piston rod:2','Piston rod:2',
'Piston rod:2',#9282,#9285,'Piston rod:2');
#249=NEXT_ASSEMBLY_USAGE_OCCURRENCE('Cap Screw - M4x16:2',
'Cap Screw - M4x16:2','Cap Screw - M4x16:2',#9282,#9286,
'Cap Screw - M4x16:2');
#250=NEXT_ASSEMBLY_USAGE_OCCURRENCE('Six-millimetre-pin rod clevis:2',
'Six-millimetre-pin rod clevis:2','Six-millimetre-pin rod clevis:2',#9282,
#9287,'Six-millimetre-pin rod clevis:2');
#251=NEXT_ASSEMBLY_USAGE_OCCURRENCE('Socket Set Screw - M4x6:2',
'Socket Set Screw - M4x6:2','Socket Set Screw - M4x6:2',#9282,#9288,
'Socket Set Screw - M4x6:2');
#252=NEXT_ASSEMBLY_USAGE_OCCURRENCE('Clevis Pin - 6x30:2',
'Clevis Pin - 6x30:2','Clevis Pin - 6x30:2',#9282,#9289,
'Clevis Pin - 6x30:2');
#253=NEXT_ASSEMBLY_USAGE_OCCURRENCE('Flat Washer - M6:2',
'Flat Washer - M6:2','Flat Washer - M6:2',#9282,#9290,
'Flat Washer - M6:2');
#254=NEXT_ASSEMBLY_USAGE_OCCURRENCE('Flat Washer - M6:3',
'Flat Washer - M6:3','Flat Washer - M6:3',#9282,#9290,
'Flat Washer - M6:3');
#255=NEXT_ASSEMBLY_USAGE_OCCURRENCE('Flat Washer - M6:4',
'Flat Washer - M6:4','Flat Washer - M6:4',#9282,#9290,
'Flat Washer - M6:4');
#256=NEXT_ASSEMBLY_USAGE_OCCURRENCE('Split Pin - 1.6x16:2',
'Split Pin - 1.6x16:2','Split Pin - 1.6x16:2',#9282,#9291,
'Split Pin - 1.6x16:2');
#257=NEXT_ASSEMBLY_USAGE_OCCURRENCE(
'Twenty millimetre bore cylinder and flow controls:1',
'Twenty millimetre bore cylinder and flow controls:1',
'Twenty millimetre bore cylinder and flow controls:1',#9260,#9261,
'Twenty millimetre bore cylinder and flow controls:1');
#258=NEXT_ASSEMBLY_USAGE_OCCURRENCE('Piston rod and clevis:1',
'Piston rod and clevis:1','Piston rod and clevis:1',#9260,#9282,
'Piston rod and clevis:1');
#259=ORIENTED_CLOSED_SHELL('',*,#4935,.F.);
#260=ORIENTED_CLOSED_SHELL('',*,#4948,.F.);
#261=BREP_WITH_VOIDS('Body1',#4934,(#259));
#262=BREP_WITH_VOIDS('Body1',#4947,(#260));
#263=CONICAL_SURFACE('',#5380,0.1,0.78539816339745);
#264=CONICAL_SURFACE('',#5382,0.25,0.321750554396641);
#265=CONICAL_SURFACE('',#5503,0.1,0.78539816339745);
#266=CONICAL_SURFACE('',#5505,0.25,0.321750554396641);
#267=CONICAL_SURFACE('',#5571,0.4,0.785398163397448);
#268=CONICAL_SURFACE('',#5575,0.41,0.785398163397448);
#269=CONICAL_SURFACE('',#5579,0.26,0.463647609000806);
#270=CONICAL_SURFACE('',#5583,0.225,0.785398163397448);
#271=CONICAL_SURFACE('',#5670,0.275,0.785398163397449);
#272=CONICAL_SURFACE('',#5681,0.47094010767585,1.0471975511966);
#273=CONICAL_SURFACE('',#5683,0.47094010767585,1.0471975511966);
#274=CONICAL_SURFACE('',#5776,0.325,0.785398163397448);
#275=CONICAL_SURFACE('',#5780,0.335,0.785398163397448);
#276=CONICAL_SURFACE('',#5784,0.21,0.463647609000806);
#277=CONICAL_SURFACE('',#5788,0.18,0.785398163397448);
#278=CONICAL_SURFACE('',#5836,0.185,0.785398163397449);
#279=CONICAL_SURFACE('',#5840,0.1625,0.785398163397449);
#280=CONICAL_SURFACE('',#5847,0.475,0.785398163397448);
#281=CONICAL_SURFACE('',#5855,0.255,0.785398163397449);
#282=SHAPE_REPRESENTATION_RELATIONSHIP('SRR','None',#9229,#310);
#283=SHAPE_REPRESENTATION_RELATIONSHIP('SRR','None',#9230,#311);
#284=SHAPE_REPRESENTATION_RELATIONSHIP('SRR','None',#9231,#312);
#285=SHAPE_REPRESENTATION_RELATIONSHIP('SRR','None',#9232,#313);
#286=SHAPE_REPRESENTATION_RELATIONSHIP('SRR','None',#9233,#314);
#287=SHAPE_REPRESENTATION_RELATIONSHIP('SRR','None',#9234,#315);
#288=SHAPE_REPRESENTATION_RELATIONSHIP('SRR','None',#9235,#316);
#289=SHAPE_REPRESENTATION_RELATIONSHIP('SRR','None',#9236,#317);
#290=SHAPE_REPRESENTATION_RELATIONSHIP('SRR','None',#9237,#318);
#291=SHAPE_REPRESENTATION_RELATIONSHIP('SRR','None',#9238,#319);
#292=SHAPE_REPRESENTATION_RELATIONSHIP('SRR','None',#9239,#320);
#293=SHAPE_REPRESENTATION_RELATIONSHIP('SRR','None',#9241,#321);
#294=SHAPE_REPRESENTATION_RELATIONSHIP('SRR','None',#9242,#322);
#295=SHAPE_REPRESENTATION_RELATIONSHIP('SRR','None',#9243,#323);
#296=SHAPE_REPRESENTATION_RELATIONSHIP('SRR','None',#9244,#324);
#297=SHAPE_REPRESENTATION_RELATIONSHIP('SRR','None',#9245,#325);
#298=SHAPE_REPRESENTATION_RELATIONSHIP('SRR','None',#9246,#326);
#299=SHAPE_REPRESENTATION_RELATIONSHIP('SRR','None',#9247,#327);
#300=SHAPE_REPRESENTATION_RELATIONSHIP('SRR','None',#9248,#328);
#301=SHAPE_REPRESENTATION_RELATIONSHIP('SRR','None',#9250,#329);
#302=SHAPE_REPRESENTATION_RELATIONSHIP('SRR','None',#9251,#330);
#303=SHAPE_REPRESENTATION_RELATIONSHIP('SRR','None',#9252,#331);
#304=SHAPE_REPRESENTATION_RELATIONSHIP('SRR','None',#9253,#332);
#305=SHAPE_REPRESENTATION_RELATIONSHIP('SRR','None',#9254,#333);
#306=SHAPE_REPRESENTATION_RELATIONSHIP('SRR','None',#9255,#334);
#307=SHAPE_REPRESENTATION_RELATIONSHIP('SRR','None',#9256,#335);
#308=SHAPE_REPRESENTATION_RELATIONSHIP('SRR','None',#9257,#336);
#309=SHAPE_REPRESENTATION_RELATIONSHIP('SRR','None',#9258,#337);
#310=ADVANCED_BREP_SHAPE_REPRESENTATION('',(#366),#9072);
#311=ADVANCED_BREP_SHAPE_REPRESENTATION('',(#367),#9073);
#312=ADVANCED_BREP_SHAPE_REPRESENTATION('',(#368),#9074);
#313=ADVANCED_BREP_SHAPE_REPRESENTATION('',(#369),#9075);
#314=ADVANCED_BREP_SHAPE_REPRESENTATION('',(#370),#9076);
#315=ADVANCED_BREP_SHAPE_REPRESENTATION('',(#371),#9077);
#316=ADVANCED_BREP_SHAPE_REPRESENTATION('',(#372),#9078);
#317=ADVANCED_BREP_SHAPE_REPRESENTATION('',(#373),#9079);
#318=ADVANCED_BREP_SHAPE_REPRESENTATION('',(#374),#9080);
#319=ADVANCED_BREP_SHAPE_REPRESENTATION('',(#375),#9081);
#320=ADVANCED_BREP_SHAPE_REPRESENTATION('',(#261),#9082);
#321=ADVANCED_BREP_SHAPE_REPRESENTATION('',(#376),#9084);
#322=ADVANCED_BREP_SHAPE_REPRESENTATION('',(#377),#9085);
#323=ADVANCED_BREP_SHAPE_REPRESENTATION('',(#378),#9086);
#324=ADVANCED_BREP_SHAPE_REPRESENTATION('',(#379),#9087);
#325=ADVANCED_BREP_SHAPE_REPRESENTATION('',(#380),#9088);
#326=ADVANCED_BREP_SHAPE_REPRESENTATION('',(#381),#9089);
#327=ADVANCED_BREP_SHAPE_REPRESENTATION('',(#382),#9090);
#328=ADVANCED_BREP_SHAPE_REPRESENTATION('',(#383),#9091);
#329=ADVANCED_BREP_SHAPE_REPRESENTATION('',(#384),#9093);
#330=ADVANCED_BREP_SHAPE_REPRESENTATION('',(#385),#9094);
#331=ADVANCED_BREP_SHAPE_REPRESENTATION('',(#386),#9095);
#332=ADVANCED_BREP_SHAPE_REPRESENTATION('',(#262),#9096);
#333=ADVANCED_BREP_SHAPE_REPRESENTATION('',(#387),#9097);
#334=ADVANCED_BREP_SHAPE_REPRESENTATION('',(#388),#9098);
#335=ADVANCED_BREP_SHAPE_REPRESENTATION('',(#389),#9099);
#336=ADVANCED_BREP_SHAPE_REPRESENTATION('',(#390),#9100);
#337=ADVANCED_BREP_SHAPE_REPRESENTATION('',(#391),#9101);
#338=STYLED_ITEM('',(#9446),#366);
#339=STYLED_ITEM('',(#9453),#367);
#340=STYLED_ITEM('',(#9467),#368);
#341=STYLED_ITEM('',(#9446),#369);
#342=STYLED_ITEM('',(#9453),#370);
#343=STYLED_ITEM('',(#9467),#371);
#344=STYLED_ITEM('',(#9453),#372);
#345=STYLED_ITEM('',(#9453),#373);
#346=STYLED_ITEM('',(#9453),#374);
#347=STYLED_ITEM('',(#9453),#375);
#348=STYLED_ITEM('',(#9467),#261);
#349=STYLED_ITEM('',(#9439),#376);
#350=STYLED_ITEM('',(#9474),#377);
#351=STYLED_ITEM('',(#9467),#378);
#352=STYLED_ITEM('',(#9460),#379);
#353=STYLED_ITEM('',(#9467),#380);
#354=STYLED_ITEM('',(#9460),#381);
#355=STYLED_ITEM('',(#9467),#382);
#356=STYLED_ITEM('',(#9467),#383);
#357=STYLED_ITEM('',(#9474),#384);
#358=STYLED_ITEM('',(#9467),#385);
#359=STYLED_ITEM('',(#9460),#386);
#360=STYLED_ITEM('',(#9467),#262);
#361=STYLED_ITEM('',(#9460),#387);
#362=STYLED_ITEM('',(#9467),#388);
#363=STYLED_ITEM('',(#9460),#389);
#364=STYLED_ITEM('',(#9467),#390);
#365=STYLED_ITEM('',(#9460),#391);
#366=MANIFOLD_SOLID_BREP('Body1',#4924);
#367=MANIFOLD_SOLID_BREP('Body1',#4925);
#368=MANIFOLD_SOLID_BREP('Body1',#4926);
#369=MANIFOLD_SOLID_BREP('Body1',#4927);
#370=MANIFOLD_SOLID_BREP('Body1',#4928);
#371=MANIFOLD_SOLID_BREP('Body1',#4929);
#372=MANIFOLD_SOLID_BREP('Body1',#4930);
#373=MANIFOLD_SOLID_BREP('Body1',#4931);
#374=MANIFOLD_SOLID_BREP('Body1',#4932);
#375=MANIFOLD_SOLID_BREP('Body1',#4933);
#376=MANIFOLD_SOLID_BREP('Body1',#4936);
#377=MANIFOLD_SOLID_BREP('Body1',#4937);
#378=MANIFOLD_SOLID_BREP('Body1',#4938);
#379=MANIFOLD_SOLID_BREP('Body1',#4939);
#380=MANIFOLD_SOLID_BREP('Body1',#4940);
#381=MANIFOLD_SOLID_BREP('Body1',#4941);
#382=MANIFOLD_SOLID_BREP('Body1',#4942);
#383=MANIFOLD_SOLID_BREP('Body1',#4943);
#384=MANIFOLD_SOLID_BREP('Body1',#4944);
#385=MANIFOLD_SOLID_BREP('Body1',#4945);
#386=MANIFOLD_SOLID_BREP('Body1',#4946);
#387=MANIFOLD_SOLID_BREP('Body1',#4949);
#388=MANIFOLD_SOLID_BREP('Body1',#4950);
#389=MANIFOLD_SOLID_BREP('Body1',#4951);
#390=MANIFOLD_SOLID_BREP('Body1',#4952);
#391=MANIFOLD_SOLID_BREP('Body1',#4953);
#392=FACE_BOUND('',#1021,.T.);
#393=FACE_BOUND('',#1028,.T.);
#394=FACE_BOUND('',#1030,.T.);
#395=FACE_BOUND('',#1031,.T.);
#396=FACE_BOUND('',#1032,.T.);
#397=FACE_BOUND('',#1033,.T.);
#398=FACE_BOUND('',#1034,.T.);
#399=FACE_BOUND('',#1037,.T.);
#400=FACE_BOUND('',#1038,.T.);
#401=FACE_BOUND('',#1039,.T.);
#402=FACE_BOUND('',#1040,.T.);
#403=FACE_BOUND('',#1041,.T.);
#404=FACE_BOUND('',#1044,.T.);
#405=FACE_BOUND('',#1046,.T.);
#406=FACE_BOUND('',#1047,.T.);
#407=FACE_BOUND('',#1050,.T.);
#408=FACE_BOUND('',#1052,.T.);
#409=FACE_BOUND('',#1056,.T.);
#410=FACE_BOUND('',#1058,.T.);
#411=FACE_BOUND('',#1062,.T.);
#412=FACE_BOUND('',#1066,.T.);
#413=FACE_BOUND('',#1070,.T.);
#414=FACE_BOUND('',#1074,.T.);
#415=FACE_BOUND('',#1085,.T.);
#416=FACE_BOUND('',#1090,.T.);
#417=FACE_BOUND('',#1113,.T.);
#418=FACE_BOUND('',#1120,.T.);
#419=FACE_BOUND('',#1121,.T.);
#420=FACE_BOUND('',#1122,.T.);
#421=FACE_BOUND('',#1123,.T.);
#422=FACE_BOUND('',#1126,.T.);
#423=FACE_BOUND('',#1127,.T.);
#424=FACE_BOUND('',#1128,.T.);
#425=FACE_BOUND('',#1129,.T.);
#426=FACE_BOUND('',#1130,.T.);
#427=FACE_BOUND('',#1133,.T.);
#428=FACE_BOUND('',#1135,.T.);
#429=FACE_BOUND('',#1136,.T.);
#430=FACE_BOUND('',#1139,.T.);
#431=FACE_BOUND('',#1141,.T.);
#432=FACE_BOUND('',#1145,.T.);
#433=FACE_BOUND('',#1147,.T.);
#434=FACE_BOUND('',#1151,.T.);
#435=FACE_BOUND('',#1155,.T.);
#436=FACE_BOUND('',#1159,.T.);
#437=FACE_BOUND('',#1163,.T.);
#438=FACE_BOUND('',#1174,.T.);
#439=FACE_BOUND('',#1179,.T.);
#440=FACE_BOUND('',#1185,.T.);
#441=FACE_BOUND('',#1187,.T.);
#442=FACE_BOUND('',#1191,.T.);
#443=FACE_BOUND('',#1193,.T.);
#444=FACE_BOUND('',#1197,.T.);
#445=FACE_BOUND('',#1199,.T.);
#446=FACE_BOUND('',#1204,.T.);
#447=FACE_BOUND('',#1207,.T.);
#448=FACE_BOUND('',#1215,.T.);
#449=FACE_BOUND('',#1216,.T.);
#450=FACE_BOUND('',#1217,.T.);
#451=FACE_BOUND('',#1218,.T.);
#452=FACE_BOUND('',#1220,.T.);
#453=FACE_BOUND('',#1221,.T.);
#454=FACE_BOUND('',#1222,.T.);
#455=FACE_BOUND('',#1223,.T.);
#456=FACE_BOUND('',#1229,.T.);
#457=FACE_BOUND('',#1244,.T.);
#458=FACE_BOUND('',#1246,.T.);
#459=FACE_BOUND('',#1248,.T.);
#460=FACE_BOUND('',#1256,.T.);
#461=FACE_BOUND('',#1259,.T.);
#462=FACE_BOUND('',#1263,.T.);
#463=FACE_BOUND('',#1266,.T.);
#464=FACE_BOUND('',#1269,.T.);
#465=FACE_BOUND('',#1272,.T.);
#466=FACE_BOUND('',#1277,.T.);
#467=FACE_BOUND('',#1279,.T.);
#468=FACE_BOUND('',#1284,.T.);
#469=FACE_BOUND('',#1286,.T.);
#470=FACE_BOUND('',#1294,.T.);
#471=FACE_BOUND('',#1297,.T.);
#472=FACE_BOUND('',#1308,.T.);
#473=FACE_BOUND('',#1310,.T.);
#474=FACE_BOUND('',#1313,.T.);
#475=FACE_BOUND('',#1316,.T.);
#476=FACE_BOUND('',#1318,.T.);
#477=FACE_BOUND('',#1323,.T.);
#478=FACE_BOUND('',#1325,.T.);
#479=FACE_BOUND('',#1331,.T.);
#480=FACE_BOUND('',#1338,.T.);
#481=FACE_BOUND('',#1357,.T.);
#482=FACE_BOUND('',#1359,.T.);
#483=FACE_BOUND('',#1361,.T.);
#484=FACE_BOUND('',#1363,.T.);
#485=FACE_BOUND('',#1368,.T.);
#486=FACE_BOUND('',#1370,.T.);
#487=FACE_BOUND('',#1372,.T.);
#488=FACE_BOUND('',#1374,.T.);
#489=FACE_BOUND('',#1383,.T.);
#490=FACE_BOUND('',#1393,.T.);
#491=FACE_BOUND('',#1395,.T.);
#492=FACE_BOUND('',#1401,.T.);
#493=FACE_BOUND('',#1403,.T.);
#494=FACE_BOUND('',#1405,.T.);
#495=ELLIPSE('',#5279,0.282842712474619,0.2);
#496=ELLIPSE('',#5280,0.282842712474619,0.2);
#497=ELLIPSE('',#5282,0.282842712474619,0.2);
#498=ELLIPSE('',#5283,0.282842712474619,0.2);
#499=ELLIPSE('',#5287,0.282842712474619,0.2);
#500=ELLIPSE('',#5289,0.282842712474619,0.2);
#501=ELLIPSE('',#5291,0.282842712474619,0.2);
#502=ELLIPSE('',#5409,0.282842712474618,0.2);
#503=ELLIPSE('',#5410,0.282842712474618,0.2);
#504=ELLIPSE('',#5411,0.282842712474618,0.2);
#505=ELLIPSE('',#5414,0.282842712474618,0.2);
#506=ELLIPSE('',#5415,0.282842712474618,0.2);
#507=ELLIPSE('',#5417,0.282842712474618,0.2);
#508=ELLIPSE('',#5418,0.282842712474618,0.2);
#509=PLANE('',#5269);
#510=PLANE('',#5273);
#511=PLANE('',#5274);
#512=PLANE('',#5276);
#513=PLANE('',#5292);
#514=PLANE('',#5294);
#515=PLANE('',#5295);
#516=PLANE('',#5297);
#517=PLANE('',#5308);
#518=PLANE('',#5312);
#519=PLANE('',#5328);
#520=PLANE('',#5329);
#521=PLANE('',#5330);
#522=PLANE('',#5331);
#523=PLANE('',#5332);
#524=PLANE('',#5333);
#525=PLANE('',#5334);
#526=PLANE('',#5339);
#527=PLANE('',#5340);
#528=PLANE('',#5348);
#529=PLANE('',#5350);
#530=PLANE('',#5355);
#531=PLANE('',#5357);
#532=PLANE('',#5358);
#533=PLANE('',#5359);
#534=PLANE('',#5360);
#535=PLANE('',#5361);
#536=PLANE('',#5362);
#537=PLANE('',#5363);
#538=PLANE('',#5364);
#539=PLANE('',#5365);
#540=PLANE('',#5367);
#541=PLANE('',#5368);
#542=PLANE('',#5369);
#543=PLANE('',#5370);
#544=PLANE('',#5371);
#545=PLANE('',#5372);
#546=PLANE('',#5373);
#547=PLANE('',#5378);
#548=PLANE('',#5386);
#549=PLANE('',#5390);
#550=PLANE('',#5395);
#551=PLANE('',#5399);
#552=PLANE('',#5400);
#553=PLANE('',#5402);
#554=PLANE('',#5404);
#555=PLANE('',#5419);
#556=PLANE('',#5421);
#557=PLANE('',#5423);
#558=PLANE('',#5425);
#559=PLANE('',#5431);
#560=PLANE('',#5437);
#561=PLANE('',#5452);
#562=PLANE('',#5453);
#563=PLANE('',#5454);
#564=PLANE('',#5455);
#565=PLANE('',#5456);
#566=PLANE('',#5457);
#567=PLANE('',#5462);
#568=PLANE('',#5463);
#569=PLANE('',#5471);
#570=PLANE('',#5473);
#571=PLANE('',#5478);
#572=PLANE('',#5480);
#573=PLANE('',#5481);
#574=PLANE('',#5482);
#575=PLANE('',#5483);
#576=PLANE('',#5484);
#577=PLANE('',#5485);
#578=PLANE('',#5486);
#579=PLANE('',#5487);
#580=PLANE('',#5488);
#581=PLANE('',#5490);
#582=PLANE('',#5491);
#583=PLANE('',#5492);
#584=PLANE('',#5493);
#585=PLANE('',#5494);
#586=PLANE('',#5495);
#587=PLANE('',#5496);
#588=PLANE('',#5501);
#589=PLANE('',#5509);
#590=PLANE('',#5513);
#591=PLANE('',#5521);
#592=PLANE('',#5522);
#593=PLANE('',#5530);
#594=PLANE('',#5531);
#595=PLANE('',#5539);
#596=PLANE('',#5540);
#597=PLANE('',#5551);
#598=PLANE('',#5556);
#599=PLANE('',#5562);
#600=PLANE('',#5563);
#601=PLANE('',#5564);
#602=PLANE('',#5565);
#603=PLANE('',#5566);
#604=PLANE('',#5567);
#605=PLANE('',#5569);
#606=PLANE('',#5577);
#607=PLANE('',#5585);
#608=PLANE('',#5586);
#609=PLANE('',#5587);
#610=PLANE('',#5588);
#611=PLANE('',#5589);
#612=PLANE('',#5590);
#613=PLANE('',#5591);
#614=PLANE('',#5592);
#615=PLANE('',#5593);
#616=PLANE('',#5599);
#617=PLANE('',#5601);
#618=PLANE('',#5603);
#619=PLANE('',#5605);
#620=PLANE('',#5606);
#621=PLANE('',#5607);
#622=PLANE('',#5608);
#623=PLANE('',#5609);
#624=PLANE('',#5610);
#625=PLANE('',#5611);
#626=PLANE('',#5615);
#627=PLANE('',#5620);
#628=PLANE('',#5624);
#629=PLANE('',#5629);
#630=PLANE('',#5633);
#631=PLANE('',#5646);
#632=PLANE('',#5648);
#633=PLANE('',#5657);
#634=PLANE('',#5658);
#635=PLANE('',#5667);
#636=PLANE('',#5668);
#637=PLANE('',#5675);
#638=PLANE('',#5679);
#639=PLANE('',#5685);
#640=PLANE('',#5686);
#641=PLANE('',#5687);
#642=PLANE('',#5691);
#643=PLANE('',#5692);
#644=PLANE('',#5693);
#645=PLANE('',#5694);
#646=PLANE('',#5695);
#647=PLANE('',#5742);
#648=PLANE('',#5747);
#649=PLANE('',#5749);
#650=PLANE('',#5757);
#651=PLANE('',#5758);
#652=PLANE('',#5767);
#653=PLANE('',#5771);
#654=PLANE('',#5772);
#655=PLANE('',#5774);
#656=PLANE('',#5782);
#657=PLANE('',#5790);
#658=PLANE('',#5791);
#659=PLANE('',#5792);
#660=PLANE('',#5793);
#661=PLANE('',#5794);
#662=PLANE('',#5795);
#663=PLANE('',#5796);
#664=PLANE('',#5797);
#665=PLANE('',#5798);
#666=PLANE('',#5806);
#667=PLANE('',#5812);
#668=PLANE('',#5816);
#669=PLANE('',#5817);
#670=PLANE('',#5818);
#671=PLANE('',#5819);
#672=PLANE('',#5820);
#673=PLANE('',#5821);
#674=PLANE('',#5822);
#675=PLANE('',#5823);
#676=PLANE('',#5824);
#677=PLANE('',#5825);
#678=PLANE('',#5827);
#679=PLANE('',#5828);
#680=PLANE('',#5829);
#681=PLANE('',#5830);
#682=PLANE('',#5831);
#683=PLANE('',#5832);
#684=PLANE('',#5833);
#685=PLANE('',#5834);
#686=PLANE('',#5842);
#687=PLANE('',#5845);
#688=PLANE('',#5851);
#689=PLANE('',#5857);
#690=PLANE('',#5865);
#691=PLANE('',#5866);
#692=PLANE('',#5871);
#693=PLANE('',#5873);
#694=PLANE('',#5877);
#695=FACE_OUTER_BOUND('',#1001,.T.);
#696=FACE_OUTER_BOUND('',#1002,.T.);
#697=FACE_OUTER_BOUND('',#1003,.T.);
#698=FACE_OUTER_BOUND('',#1004,.T.);
#699=FACE_OUTER_BOUND('',#1005,.T.);
#700=FACE_OUTER_BOUND('',#1006,.T.);
#701=FACE_OUTER_BOUND('',#1007,.T.);
#702=FACE_OUTER_BOUND('',#1008,.T.);
#703=FACE_OUTER_BOUND('',#1009,.T.);
#704=FACE_OUTER_BOUND('',#1010,.T.);
#705=FACE_OUTER_BOUND('',#1011,.T.);
#706=FACE_OUTER_BOUND('',#1012,.T.);
#707=FACE_OUTER_BOUND('',#1013,.T.);
#708=FACE_OUTER_BOUND('',#1014,.T.);
#709=FACE_OUTER_BOUND('',#1015,.T.);
#710=FACE_OUTER_BOUND('',#1016,.T.);
#711=FACE_OUTER_BOUND('',#1017,.T.);
#712=FACE_OUTER_BOUND('',#1018,.T.);
#713=FACE_OUTER_BOUND('',#1019,.T.);
#714=FACE_OUTER_BOUND('',#1020,.T.);
#715=FACE_OUTER_BOUND('',#1022,.T.);
#716=FACE_OUTER_BOUND('',#1023,.T.);
#717=FACE_OUTER_BOUND('',#1024,.T.);
#718=FACE_OUTER_BOUND('',#1025,.T.);
#719=FACE_OUTER_BOUND('',#1026,.T.);
#720=FACE_OUTER_BOUND('',#1027,.T.);
#721=FACE_OUTER_BOUND('',#1029,.T.);
#722=FACE_OUTER_BOUND('',#1035,.T.);
#723=FACE_OUTER_BOUND('',#1036,.T.);
#724=FACE_OUTER_BOUND('',#1042,.T.);
#725=FACE_OUTER_BOUND('',#1043,.T.);
#726=FACE_OUTER_BOUND('',#1045,.T.);
#727=FACE_OUTER_BOUND('',#1048,.T.);
#728=FACE_OUTER_BOUND('',#1049,.T.);
#729=FACE_OUTER_BOUND('',#1051,.T.);
#730=FACE_OUTER_BOUND('',#1053,.T.);
#731=FACE_OUTER_BOUND('',#1054,.T.);
#732=FACE_OUTER_BOUND('',#1055,.T.);
#733=FACE_OUTER_BOUND('',#1057,.T.);
#734=FACE_OUTER_BOUND('',#1059,.T.);
#735=FACE_OUTER_BOUND('',#1060,.T.);
#736=FACE_OUTER_BOUND('',#1061,.T.);
#737=FACE_OUTER_BOUND('',#1063,.T.);
#738=FACE_OUTER_BOUND('',#1064,.T.);
#739=FACE_OUTER_BOUND('',#1065,.T.);
#740=FACE_OUTER_BOUND('',#1067,.T.);
#741=FACE_OUTER_BOUND('',#1068,.T.);
#742=FACE_OUTER_BOUND('',#1069,.T.);
#743=FACE_OUTER_BOUND('',#1071,.T.);
#744=FACE_OUTER_BOUND('',#1072,.T.);
#745=FACE_OUTER_BOUND('',#1073,.T.);
#746=FACE_OUTER_BOUND('',#1075,.T.);
#747=FACE_OUTER_BOUND('',#1076,.T.);
#748=FACE_OUTER_BOUND('',#1077,.T.);
#749=FACE_OUTER_BOUND('',#1078,.T.);
#750=FACE_OUTER_BOUND('',#1079,.T.);
#751=FACE_OUTER_BOUND('',#1080,.T.);
#752=FACE_OUTER_BOUND('',#1081,.T.);
#753=FACE_OUTER_BOUND('',#1082,.T.);
#754=FACE_OUTER_BOUND('',#1083,.T.);
#755=FACE_OUTER_BOUND('',#1084,.T.);
#756=FACE_OUTER_BOUND('',#1086,.T.);
#757=FACE_OUTER_BOUND('',#1087,.T.);
#758=FACE_OUTER_BOUND('',#1088,.T.);
#759=FACE_OUTER_BOUND('',#1089,.T.);
#760=FACE_OUTER_BOUND('',#1091,.T.);
#761=FACE_OUTER_BOUND('',#1092,.T.);
#762=FACE_OUTER_BOUND('',#1093,.T.);
#763=FACE_OUTER_BOUND('',#1094,.T.);
#764=FACE_OUTER_BOUND('',#1095,.T.);
#765=FACE_OUTER_BOUND('',#1096,.T.);
#766=FACE_OUTER_BOUND('',#1097,.T.);
#767=FACE_OUTER_BOUND('',#1098,.T.);
#768=FACE_OUTER_BOUND('',#1099,.T.);
#769=FACE_OUTER_BOUND('',#1100,.T.);
#770=FACE_OUTER_BOUND('',#1101,.T.);
#771=FACE_OUTER_BOUND('',#1102,.T.);
#772=FACE_OUTER_BOUND('',#1103,.T.);
#773=FACE_OUTER_BOUND('',#1104,.T.);
#774=FACE_OUTER_BOUND('',#1105,.T.);
#775=FACE_OUTER_BOUND('',#1106,.T.);
#776=FACE_OUTER_BOUND('',#1107,.T.);
#777=FACE_OUTER_BOUND('',#1108,.T.);
#778=FACE_OUTER_BOUND('',#1109,.T.);
#779=FACE_OUTER_BOUND('',#1110,.T.);
#780=FACE_OUTER_BOUND('',#1111,.T.);
#781=FACE_OUTER_BOUND('',#1112,.T.);
#782=FACE_OUTER_BOUND('',#1114,.T.);
#783=FACE_OUTER_BOUND('',#1115,.T.);
#784=FACE_OUTER_BOUND('',#1116,.T.);
#785=FACE_OUTER_BOUND('',#1117,.T.);
#786=FACE_OUTER_BOUND('',#1118,.T.);
#787=FACE_OUTER_BOUND('',#1119,.T.);
#788=FACE_OUTER_BOUND('',#1124,.T.);
#789=FACE_OUTER_BOUND('',#1125,.T.);
#790=FACE_OUTER_BOUND('',#1131,.T.);
#791=FACE_OUTER_BOUND('',#1132,.T.);
#792=FACE_OUTER_BOUND('',#1134,.T.);
#793=FACE_OUTER_BOUND('',#1137,.T.);
#794=FACE_OUTER_BOUND('',#1138,.T.);
#795=FACE_OUTER_BOUND('',#1140,.T.);
#796=FACE_OUTER_BOUND('',#1142,.T.);
#797=FACE_OUTER_BOUND('',#1143,.T.);
#798=FACE_OUTER_BOUND('',#1144,.T.);
#799=FACE_OUTER_BOUND('',#1146,.T.);
#800=FACE_OUTER_BOUND('',#1148,.T.);
#801=FACE_OUTER_BOUND('',#1149,.T.);
#802=FACE_OUTER_BOUND('',#1150,.T.);
#803=FACE_OUTER_BOUND('',#1152,.T.);
#804=FACE_OUTER_BOUND('',#1153,.T.);
#805=FACE_OUTER_BOUND('',#1154,.T.);
#806=FACE_OUTER_BOUND('',#1156,.T.);
#807=FACE_OUTER_BOUND('',#1157,.T.);
#808=FACE_OUTER_BOUND('',#1158,.T.);
#809=FACE_OUTER_BOUND('',#1160,.T.);
#810=FACE_OUTER_BOUND('',#1161,.T.);
#811=FACE_OUTER_BOUND('',#1162,.T.);
#812=FACE_OUTER_BOUND('',#1164,.T.);
#813=FACE_OUTER_BOUND('',#1165,.T.);
#814=FACE_OUTER_BOUND('',#1166,.T.);
#815=FACE_OUTER_BOUND('',#1167,.T.);
#816=FACE_OUTER_BOUND('',#1168,.T.);
#817=FACE_OUTER_BOUND('',#1169,.T.);
#818=FACE_OUTER_BOUND('',#1170,.T.);
#819=FACE_OUTER_BOUND('',#1171,.T.);
#820=FACE_OUTER_BOUND('',#1172,.T.);
#821=FACE_OUTER_BOUND('',#1173,.T.);
#822=FACE_OUTER_BOUND('',#1175,.T.);
#823=FACE_OUTER_BOUND('',#1176,.T.);
#824=FACE_OUTER_BOUND('',#1177,.T.);
#825=FACE_OUTER_BOUND('',#1178,.T.);
#826=FACE_OUTER_BOUND('',#1180,.T.);
#827=FACE_OUTER_BOUND('',#1181,.T.);
#828=FACE_OUTER_BOUND('',#1182,.T.);
#829=FACE_OUTER_BOUND('',#1183,.T.);
#830=FACE_OUTER_BOUND('',#1184,.T.);
#831=FACE_OUTER_BOUND('',#1186,.T.);
#832=FACE_OUTER_BOUND('',#1188,.T.);
#833=FACE_OUTER_BOUND('',#1189,.T.);
#834=FACE_OUTER_BOUND('',#1190,.T.);
#835=FACE_OUTER_BOUND('',#1192,.T.);
#836=FACE_OUTER_BOUND('',#1194,.T.);
#837=FACE_OUTER_BOUND('',#1195,.T.);
#838=FACE_OUTER_BOUND('',#1196,.T.);
#839=FACE_OUTER_BOUND('',#1198,.T.);
#840=FACE_OUTER_BOUND('',#1200,.T.);
#841=FACE_OUTER_BOUND('',#1201,.T.);
#842=FACE_OUTER_BOUND('',#1202,.T.);
#843=FACE_OUTER_BOUND('',#1203,.T.);
#844=FACE_OUTER_BOUND('',#1205,.T.);
#845=FACE_OUTER_BOUND('',#1206,.T.);
#846=FACE_OUTER_BOUND('',#1208,.T.);
#847=FACE_OUTER_BOUND('',#1209,.T.);
#848=FACE_OUTER_BOUND('',#1210,.T.);
#849=FACE_OUTER_BOUND('',#1211,.T.);
#850=FACE_OUTER_BOUND('',#1212,.T.);
#851=FACE_OUTER_BOUND('',#1213,.T.);
#852=FACE_OUTER_BOUND('',#1214,.T.);
#853=FACE_OUTER_BOUND('',#1219,.T.);
#854=FACE_OUTER_BOUND('',#1224,.T.);
#855=FACE_OUTER_BOUND('',#1225,.T.);
#856=FACE_OUTER_BOUND('',#1226,.T.);
#857=FACE_OUTER_BOUND('',#1227,.T.);
#858=FACE_OUTER_BOUND('',#1228,.T.);
#859=FACE_OUTER_BOUND('',#1230,.T.);
#860=FACE_OUTER_BOUND('',#1231,.T.);
#861=FACE_OUTER_BOUND('',#1232,.T.);
#862=FACE_OUTER_BOUND('',#1233,.T.);
#863=FACE_OUTER_BOUND('',#1234,.T.);
#864=FACE_OUTER_BOUND('',#1235,.T.);
#865=FACE_OUTER_BOUND('',#1236,.T.);
#866=FACE_OUTER_BOUND('',#1237,.T.);
#867=FACE_OUTER_BOUND('',#1238,.T.);
#868=FACE_OUTER_BOUND('',#1239,.T.);
#869=FACE_OUTER_BOUND('',#1240,.T.);
#870=FACE_OUTER_BOUND('',#1241,.T.);
#871=FACE_OUTER_BOUND('',#1242,.T.);
#872=FACE_OUTER_BOUND('',#1243,.T.);
#873=FACE_OUTER_BOUND('',#1245,.T.);
#874=FACE_OUTER_BOUND('',#1247,.T.);
#875=FACE_OUTER_BOUND('',#1249,.T.);
#876=FACE_OUTER_BOUND('',#1250,.T.);
#877=FACE_OUTER_BOUND('',#1251,.T.);
#878=FACE_OUTER_BOUND('',#1252,.T.);
#879=FACE_OUTER_BOUND('',#1253,.T.);
#880=FACE_OUTER_BOUND('',#1254,.T.);
#881=FACE_OUTER_BOUND('',#1255,.T.);
#882=FACE_OUTER_BOUND('',#1257,.T.);
#883=FACE_OUTER_BOUND('',#1258,.T.);
#884=FACE_OUTER_BOUND('',#1260,.T.);
#885=FACE_OUTER_BOUND('',#1261,.T.);
#886=FACE_OUTER_BOUND('',#1262,.T.);
#887=FACE_OUTER_BOUND('',#1264,.T.);
#888=FACE_OUTER_BOUND('',#1265,.T.);
#889=FACE_OUTER_BOUND('',#1267,.T.);
#890=FACE_OUTER_BOUND('',#1268,.T.);
#891=FACE_OUTER_BOUND('',#1270,.T.);
#892=FACE_OUTER_BOUND('',#1271,.T.);
#893=FACE_OUTER_BOUND('',#1273,.T.);
#894=FACE_OUTER_BOUND('',#1274,.T.);
#895=FACE_OUTER_BOUND('',#1275,.T.);
#896=FACE_OUTER_BOUND('',#1276,.T.);
#897=FACE_OUTER_BOUND('',#1278,.T.);
#898=FACE_OUTER_BOUND('',#1280,.T.);
#899=FACE_OUTER_BOUND('',#1281,.T.);
#900=FACE_OUTER_BOUND('',#1282,.T.);
#901=FACE_OUTER_BOUND('',#1283,.T.);
#902=FACE_OUTER_BOUND('',#1285,.T.);
#903=FACE_OUTER_BOUND('',#1287,.T.);
#904=FACE_OUTER_BOUND('',#1288,.T.);
#905=FACE_OUTER_BOUND('',#1289,.T.);
#906=FACE_OUTER_BOUND('',#1290,.T.);
#907=FACE_OUTER_BOUND('',#1291,.T.);
#908=FACE_OUTER_BOUND('',#1292,.T.);
#909=FACE_OUTER_BOUND('',#1293,.T.);
#910=FACE_OUTER_BOUND('',#1295,.T.);
#911=FACE_OUTER_BOUND('',#1296,.T.);
#912=FACE_OUTER_BOUND('',#1298,.T.);
#913=FACE_OUTER_BOUND('',#1299,.T.);
#914=FACE_OUTER_BOUND('',#1300,.T.);
#915=FACE_OUTER_BOUND('',#1301,.T.);
#916=FACE_OUTER_BOUND('',#1302,.T.);
#917=FACE_OUTER_BOUND('',#1303,.T.);
#918=FACE_OUTER_BOUND('',#1304,.T.);
#919=FACE_OUTER_BOUND('',#1305,.T.);
#920=FACE_OUTER_BOUND('',#1306,.T.);
#921=FACE_OUTER_BOUND('',#1307,.T.);
#922=FACE_OUTER_BOUND('',#1309,.T.);
#923=FACE_OUTER_BOUND('',#1311,.T.);
#924=FACE_OUTER_BOUND('',#1312,.T.);
#925=FACE_OUTER_BOUND('',#1314,.T.);
#926=FACE_OUTER_BOUND('',#1315,.T.);
#927=FACE_OUTER_BOUND('',#1317,.T.);
#928=FACE_OUTER_BOUND('',#1319,.T.);
#929=FACE_OUTER_BOUND('',#1320,.T.);
#930=FACE_OUTER_BOUND('',#1321,.T.);
#931=FACE_OUTER_BOUND('',#1322,.T.);
#932=FACE_OUTER_BOUND('',#1324,.T.);
#933=FACE_OUTER_BOUND('',#1326,.T.);
#934=FACE_OUTER_BOUND('',#1327,.T.);
#935=FACE_OUTER_BOUND('',#1328,.T.);
#936=FACE_OUTER_BOUND('',#1329,.T.);
#937=FACE_OUTER_BOUND('',#1330,.T.);
#938=FACE_OUTER_BOUND('',#1332,.T.);
#939=FACE_OUTER_BOUND('',#1333,.T.);
#940=FACE_OUTER_BOUND('',#1334,.T.);
#941=FACE_OUTER_BOUND('',#1335,.T.);
#942=FACE_OUTER_BOUND('',#1336,.T.);
#943=FACE_OUTER_BOUND('',#1337,.T.);
#944=FACE_OUTER_BOUND('',#1339,.T.);
#945=FACE_OUTER_BOUND('',#1340,.T.);
#946=FACE_OUTER_BOUND('',#1341,.T.);
#947=FACE_OUTER_BOUND('',#1342,.T.);
#948=FACE_OUTER_BOUND('',#1343,.T.);
#949=FACE_OUTER_BOUND('',#1344,.T.);
#950=FACE_OUTER_BOUND('',#1345,.T.);
#951=FACE_OUTER_BOUND('',#1346,.T.);
#952=FACE_OUTER_BOUND('',#1347,.T.);
#953=FACE_OUTER_BOUND('',#1348,.T.);
#954=FACE_OUTER_BOUND('',#1349,.T.);
#955=FACE_OUTER_BOUND('',#1350,.T.);
#956=FACE_OUTER_BOUND('',#1351,.T.);
#957=FACE_OUTER_BOUND('',#1352,.T.);
#958=FACE_OUTER_BOUND('',#1353,.T.);
#959=FACE_OUTER_BOUND('',#1354,.T.);
#960=FACE_OUTER_BOUND('',#1355,.T.);
#961=FACE_OUTER_BOUND('',#1356,.T.);
#962=FACE_OUTER_BOUND('',#1358,.T.);
#963=FACE_OUTER_BOUND('',#1360,.T.);
#964=FACE_OUTER_BOUND('',#1362,.T.);
#965=FACE_OUTER_BOUND('',#1364,.T.);
#966=FACE_OUTER_BOUND('',#1365,.T.);
#967=FACE_OUTER_BOUND('',#1366,.T.);
#968=FACE_OUTER_BOUND('',#1367,.T.);
#969=FACE_OUTER_BOUND('',#1369,.T.);
#970=FACE_OUTER_BOUND('',#1371,.T.);
#971=FACE_OUTER_BOUND('',#1373,.T.);
#972=FACE_OUTER_BOUND('',#1375,.T.);
#973=FACE_OUTER_BOUND('',#1376,.T.);
#974=FACE_OUTER_BOUND('',#1377,.T.);
#975=FACE_OUTER_BOUND('',#1378,.T.);
#976=FACE_OUTER_BOUND('',#1379,.T.);
#977=FACE_OUTER_BOUND('',#1380,.T.);
#978=FACE_OUTER_BOUND('',#1381,.T.);
#979=FACE_OUTER_BOUND('',#1382,.T.);
#980=FACE_OUTER_BOUND('',#1384,.T.);
#981=FACE_OUTER_BOUND('',#1385,.T.);
#982=FACE_OUTER_BOUND('',#1386,.T.);
#983=FACE_OUTER_BOUND('',#1387,.T.);
#984=FACE_OUTER_BOUND('',#1388,.T.);
#985=FACE_OUTER_BOUND('',#1389,.T.);
#986=FACE_OUTER_BOUND('',#1390,.T.);
#987=FACE_OUTER_BOUND('',#1391,.T.);
#988=FACE_OUTER_BOUND('',#1392,.T.);
#989=FACE_OUTER_BOUND('',#1394,.T.);
#990=FACE_OUTER_BOUND('',#1396,.T.);
#991=FACE_OUTER_BOUND('',#1397,.T.);
#992=FACE_OUTER_BOUND('',#1398,.T.);
#993=FACE_OUTER_BOUND('',#1399,.T.);
#994=FACE_OUTER_BOUND('',#1400,.T.);
#995=FACE_OUTER_BOUND('',#1402,.T.);
#996=FACE_OUTER_BOUND('',#1404,.T.);
#997=FACE_OUTER_BOUND('',#1406,.T.);
#998=FACE_OUTER_BOUND('',#1407,.T.);
#999=FACE_OUTER_BOUND('',#1408,.T.);
#1000=FACE_OUTER_BOUND('',#1409,.T.);
#1001=EDGE_LOOP('',(#3315,#3316,#3317,#3318));
#1002=EDGE_LOOP('',(#3319));
#1003=EDGE_LOOP('',(#3320,#3321,#3322,#3323));
#1004=EDGE_LOOP('',(#3324));
#1005=EDGE_LOOP('',(#3325,#3326));
#1006=EDGE_LOOP('',(#3327,#3328));
#1007=EDGE_LOOP('',(#3329,#3330,#3331));
#1008=EDGE_LOOP('',(#3332,#3333,#3334,#3335,#3336,#3337,#3338,#3339,#3340,
#3341,#3342,#3343,#3344));
#1009=EDGE_LOOP('',(#3345,#3346,#3347));
#1010=EDGE_LOOP('',(#3348,#3349));
#1011=EDGE_LOOP('',(#3350,#3351));
#1012=EDGE_LOOP('',(#3352,#3353));
#1013=EDGE_LOOP('',(#3354,#3355));
#1014=EDGE_LOOP('',(#3356,#3357,#3358));
#1015=EDGE_LOOP('',(#3359,#3360,#3361,#3362,#3363,#3364,#3365,#3366,#3367));
#1016=EDGE_LOOP('',(#3368,#3369,#3370));
#1017=EDGE_LOOP('',(#3371,#3372,#3373,#3374,#3375,#3376,#3377,#3378));
#1018=EDGE_LOOP('',(#3379,#3380));
#1019=EDGE_LOOP('',(#3381,#3382,#3383,#3384));
#1020=EDGE_LOOP('',(#3385));
#1021=EDGE_LOOP('',(#3386));
#1022=EDGE_LOOP('',(#3387,#3388,#3389,#3390));
#1023=EDGE_LOOP('',(#3391,#3392,#3393,#3394));
#1024=EDGE_LOOP('',(#3395,#3396,#3397,#3398));
#1025=EDGE_LOOP('',(#3399,#3400,#3401,#3402));
#1026=EDGE_LOOP('',(#3403,#3404,#3405,#3406));
#1027=EDGE_LOOP('',(#3407,#3408,#3409,#3410));
#1028=EDGE_LOOP('',(#3411));
#1029=EDGE_LOOP('',(#3412,#3413,#3414,#3415));
#1030=EDGE_LOOP('',(#3416));
#1031=EDGE_LOOP('',(#3417));
#1032=EDGE_LOOP('',(#3418));
#1033=EDGE_LOOP('',(#3419));
#1034=EDGE_LOOP('',(#3420));
#1035=EDGE_LOOP('',(#3421,#3422,#3423,#3424));
#1036=EDGE_LOOP('',(#3425,#3426,#3427,#3428));
#1037=EDGE_LOOP('',(#3429));
#1038=EDGE_LOOP('',(#3430));
#1039=EDGE_LOOP('',(#3431));
#1040=EDGE_LOOP('',(#3432));
#1041=EDGE_LOOP('',(#3433));
#1042=EDGE_LOOP('',(#3434,#3435,#3436,#3437));
#1043=EDGE_LOOP('',(#3438,#3439,#3440,#3441));
#1044=EDGE_LOOP('',(#3442));
#1045=EDGE_LOOP('',(#3443,#3444,#3445,#3446));
#1046=EDGE_LOOP('',(#3447));
#1047=EDGE_LOOP('',(#3448));
#1048=EDGE_LOOP('',(#3449,#3450,#3451,#3452));
#1049=EDGE_LOOP('',(#3453));
#1050=EDGE_LOOP('',(#3454,#3455,#3456,#3457));
#1051=EDGE_LOOP('',(#3458,#3459));
#1052=EDGE_LOOP('',(#3460));
#1053=EDGE_LOOP('',(#3461,#3462,#3463,#3464));
#1054=EDGE_LOOP('',(#3465,#3466,#3467,#3468));
#1055=EDGE_LOOP('',(#3469));
#1056=EDGE_LOOP('',(#3470));
#1057=EDGE_LOOP('',(#3471));
#1058=EDGE_LOOP('',(#3472));
#1059=EDGE_LOOP('',(#3473,#3474,#3475,#3476));
#1060=EDGE_LOOP('',(#3477,#3478,#3479,#3480));
#1061=EDGE_LOOP('',(#3481,#3482));
#1062=EDGE_LOOP('',(#3483));
#1063=EDGE_LOOP('',(#3484,#3485,#3486,#3487,#3488,#3489));
#1064=EDGE_LOOP('',(#3490,#3491,#3492,#3493));
#1065=EDGE_LOOP('',(#3494,#3495,#3496,#3497,#3498,#3499));
#1066=EDGE_LOOP('',(#3500));
#1067=EDGE_LOOP('',(#3501,#3502,#3503,#3504));
#1068=EDGE_LOOP('',(#3505,#3506,#3507,#3508,#3509,#3510));
#1069=EDGE_LOOP('',(#3511,#3512,#3513,#3514));
#1070=EDGE_LOOP('',(#3515));
#1071=EDGE_LOOP('',(#3516,#3517,#3518,#3519,#3520,#3521));
#1072=EDGE_LOOP('',(#3522,#3523,#3524));
#1073=EDGE_LOOP('',(#3525,#3526,#3527,#3528,#3529,#3530));
#1074=EDGE_LOOP('',(#3531));
#1075=EDGE_LOOP('',(#3532,#3533,#3534,#3535));
#1076=EDGE_LOOP('',(#3536,#3537,#3538,#3539,#3540));
#1077=EDGE_LOOP('',(#3541,#3542,#3543,#3544,#3545));
#1078=EDGE_LOOP('',(#3546,#3547,#3548,#3549));
#1079=EDGE_LOOP('',(#3550,#3551,#3552,#3553,#3554));
#1080=EDGE_LOOP('',(#3555,#3556,#3557,#3558,#3559));
#1081=EDGE_LOOP('',(#3560,#3561,#3562));
#1082=EDGE_LOOP('',(#3563,#3564,#3565,#3566));
#1083=EDGE_LOOP('',(#3567,#3568,#3569,#3570));
#1084=EDGE_LOOP('',(#3571));
#1085=EDGE_LOOP('',(#3572));
#1086=EDGE_LOOP('',(#3573,#3574,#3575));
#1087=EDGE_LOOP('',(#3576,#3577,#3578,#3579));
#1088=EDGE_LOOP('',(#3580,#3581,#3582,#3583));
#1089=EDGE_LOOP('',(#3584));
#1090=EDGE_LOOP('',(#3585));
#1091=EDGE_LOOP('',(#3586,#3587,#3588,#3589));
#1092=EDGE_LOOP('',(#3590));
#1093=EDGE_LOOP('',(#3591,#3592,#3593,#3594));
#1094=EDGE_LOOP('',(#3595));
#1095=EDGE_LOOP('',(#3596,#3597,#3598,#3599));
#1096=EDGE_LOOP('',(#3600));
#1097=EDGE_LOOP('',(#3601,#3602));
#1098=EDGE_LOOP('',(#3603,#3604));
#1099=EDGE_LOOP('',(#3605,#3606));
#1100=EDGE_LOOP('',(#3607,#3608,#3609,#3610,#3611,#3612,#3613,#3614,#3615,
#3616,#3617,#3618,#3619));
#1101=EDGE_LOOP('',(#3620,#3621,#3622));
#1102=EDGE_LOOP('',(#3623,#3624,#3625));
#1103=EDGE_LOOP('',(#3626,#3627));
#1104=EDGE_LOOP('',(#3628,#3629));
#1105=EDGE_LOOP('',(#3630,#3631));
#1106=EDGE_LOOP('',(#3632,#3633));
#1107=EDGE_LOOP('',(#3634,#3635,#3636));
#1108=EDGE_LOOP('',(#3637,#3638,#3639));
#1109=EDGE_LOOP('',(#3640,#3641,#3642,#3643,#3644,#3645,#3646,#3647,#3648));
#1110=EDGE_LOOP('',(#3649,#3650,#3651,#3652));
#1111=EDGE_LOOP('',(#3653,#3654,#3655,#3656));
#1112=EDGE_LOOP('',(#3657));
#1113=EDGE_LOOP('',(#3658));
#1114=EDGE_LOOP('',(#3659,#3660,#3661,#3662));
#1115=EDGE_LOOP('',(#3663,#3664,#3665,#3666));
#1116=EDGE_LOOP('',(#3667,#3668,#3669,#3670));
#1117=EDGE_LOOP('',(#3671,#3672,#3673,#3674));
#1118=EDGE_LOOP('',(#3675,#3676,#3677,#3678,#3679,#3680,#3681,#3682));
#1119=EDGE_LOOP('',(#3683,#3684,#3685,#3686));
#1120=EDGE_LOOP('',(#3687));
#1121=EDGE_LOOP('',(#3688));
#1122=EDGE_LOOP('',(#3689));
#1123=EDGE_LOOP('',(#3690));
#1124=EDGE_LOOP('',(#3691,#3692,#3693,#3694));
#1125=EDGE_LOOP('',(#3695,#3696,#3697,#3698));
#1126=EDGE_LOOP('',(#3699));
#1127=EDGE_LOOP('',(#3700));
#1128=EDGE_LOOP('',(#3701));
#1129=EDGE_LOOP('',(#3702));
#1130=EDGE_LOOP('',(#3703));
#1131=EDGE_LOOP('',(#3704,#3705,#3706,#3707));
#1132=EDGE_LOOP('',(#3708,#3709,#3710,#3711));
#1133=EDGE_LOOP('',(#3712));
#1134=EDGE_LOOP('',(#3713,#3714,#3715,#3716));
#1135=EDGE_LOOP('',(#3717));
#1136=EDGE_LOOP('',(#3718));
#1137=EDGE_LOOP('',(#3719,#3720,#3721,#3722));
#1138=EDGE_LOOP('',(#3723));
#1139=EDGE_LOOP('',(#3724,#3725,#3726,#3727));
#1140=EDGE_LOOP('',(#3728,#3729));
#1141=EDGE_LOOP('',(#3730));
#1142=EDGE_LOOP('',(#3731,#3732,#3733,#3734));
#1143=EDGE_LOOP('',(#3735,#3736,#3737,#3738));
#1144=EDGE_LOOP('',(#3739));
#1145=EDGE_LOOP('',(#3740));
#1146=EDGE_LOOP('',(#3741));
#1147=EDGE_LOOP('',(#3742));
#1148=EDGE_LOOP('',(#3743,#3744,#3745,#3746));
#1149=EDGE_LOOP('',(#3747,#3748,#3749,#3750));
#1150=EDGE_LOOP('',(#3751,#3752));
#1151=EDGE_LOOP('',(#3753));
#1152=EDGE_LOOP('',(#3754,#3755,#3756,#3757,#3758,#3759));
#1153=EDGE_LOOP('',(#3760,#3761,#3762,#3763));
#1154=EDGE_LOOP('',(#3764,#3765,#3766,#3767,#3768,#3769));
#1155=EDGE_LOOP('',(#3770));
#1156=EDGE_LOOP('',(#3771,#3772,#3773,#3774));
#1157=EDGE_LOOP('',(#3775,#3776,#3777,#3778,#3779,#3780));
#1158=EDGE_LOOP('',(#3781,#3782,#3783,#3784));
#1159=EDGE_LOOP('',(#3785));
#1160=EDGE_LOOP('',(#3786,#3787,#3788,#3789,#3790,#3791));
#1161=EDGE_LOOP('',(#3792,#3793,#3794));
#1162=EDGE_LOOP('',(#3795,#3796,#3797,#3798,#3799,#3800));
#1163=EDGE_LOOP('',(#3801));
#1164=EDGE_LOOP('',(#3802,#3803,#3804,#3805));
#1165=EDGE_LOOP('',(#3806,#3807,#3808,#3809,#3810));
#1166=EDGE_LOOP('',(#3811,#3812,#3813,#3814,#3815));
#1167=EDGE_LOOP('',(#3816,#3817,#3818,#3819));
#1168=EDGE_LOOP('',(#3820,#3821,#3822,#3823,#3824));
#1169=EDGE_LOOP('',(#3825,#3826,#3827,#3828,#3829));
#1170=EDGE_LOOP('',(#3830,#3831,#3832));
#1171=EDGE_LOOP('',(#3833,#3834,#3835,#3836));
#1172=EDGE_LOOP('',(#3837,#3838,#3839,#3840));
#1173=EDGE_LOOP('',(#3841));
#1174=EDGE_LOOP('',(#3842));
#1175=EDGE_LOOP('',(#3843,#3844,#3845));
#1176=EDGE_LOOP('',(#3846,#3847,#3848,#3849));
#1177=EDGE_LOOP('',(#3850,#3851,#3852,#3853));
#1178=EDGE_LOOP('',(#3854));
#1179=EDGE_LOOP('',(#3855));
#1180=EDGE_LOOP('',(#3856,#3857,#3858,#3859));
#1181=EDGE_LOOP('',(#3860));
#1182=EDGE_LOOP('',(#3861,#3862,#3863,#3864));
#1183=EDGE_LOOP('',(#3865,#3866,#3867,#3868));
#1184=EDGE_LOOP('',(#3869));
#1185=EDGE_LOOP('',(#3870));
#1186=EDGE_LOOP('',(#3871));
#1187=EDGE_LOOP('',(#3872));
#1188=EDGE_LOOP('',(#3873,#3874,#3875,#3876));
#1189=EDGE_LOOP('',(#3877,#3878,#3879,#3880));
#1190=EDGE_LOOP('',(#3881));
#1191=EDGE_LOOP('',(#3882));
#1192=EDGE_LOOP('',(#3883));
#1193=EDGE_LOOP('',(#3884));
#1194=EDGE_LOOP('',(#3885,#3886,#3887,#3888));
#1195=EDGE_LOOP('',(#3889,#3890,#3891,#3892));
#1196=EDGE_LOOP('',(#3893));
#1197=EDGE_LOOP('',(#3894));
#1198=EDGE_LOOP('',(#3895));
#1199=EDGE_LOOP('',(#3896));
#1200=EDGE_LOOP('',(#3897,#3898,#3899,#3900));
#1201=EDGE_LOOP('',(#3901,#3902,#3903,#3904));
#1202=EDGE_LOOP('',(#3905,#3906,#3907,#3908));
#1203=EDGE_LOOP('',(#3909));
#1204=EDGE_LOOP('',(#3910));
#1205=EDGE_LOOP('',(#3911,#3912,#3913,#3914));
#1206=EDGE_LOOP('',(#3915));
#1207=EDGE_LOOP('',(#3916));
#1208=EDGE_LOOP('',(#3917,#3918,#3919,#3920));
#1209=EDGE_LOOP('',(#3921,#3922,#3923,#3924));
#1210=EDGE_LOOP('',(#3925,#3926,#3927,#3928));
#1211=EDGE_LOOP('',(#3929,#3930,#3931,#3932));
#1212=EDGE_LOOP('',(#3933,#3934,#3935,#3936));
#1213=EDGE_LOOP('',(#3937,#3938,#3939,#3940));
#1214=EDGE_LOOP('',(#3941,#3942,#3943,#3944));
#1215=EDGE_LOOP('',(#3945));
#1216=EDGE_LOOP('',(#3946));
#1217=EDGE_LOOP('',(#3947));
#1218=EDGE_LOOP('',(#3948));
#1219=EDGE_LOOP('',(#3949,#3950,#3951,#3952));
#1220=EDGE_LOOP('',(#3953));
#1221=EDGE_LOOP('',(#3954));
#1222=EDGE_LOOP('',(#3955));
#1223=EDGE_LOOP('',(#3956));
#1224=EDGE_LOOP('',(#3957));
#1225=EDGE_LOOP('',(#3958,#3959,#3960,#3961));
#1226=EDGE_LOOP('',(#3962,#3963,#3964,#3965));
#1227=EDGE_LOOP('',(#3966,#3967,#3968,#3969));
#1228=EDGE_LOOP('',(#3970));
#1229=EDGE_LOOP('',(#3971));
#1230=EDGE_LOOP('',(#3972,#3973,#3974,#3975));
#1231=EDGE_LOOP('',(#3976,#3977,#3978,#3979));
#1232=EDGE_LOOP('',(#3980,#3981,#3982,#3983));
#1233=EDGE_LOOP('',(#3984));
#1234=EDGE_LOOP('',(#3985,#3986,#3987,#3988));
#1235=EDGE_LOOP('',(#3989,#3990,#3991,#3992));
#1236=EDGE_LOOP('',(#3993,#3994,#3995,#3996));
#1237=EDGE_LOOP('',(#3997,#3998,#3999,#4000));
#1238=EDGE_LOOP('',(#4001,#4002,#4003,#4004));
#1239=EDGE_LOOP('',(#4005,#4006,#4007,#4008));
#1240=EDGE_LOOP('',(#4009,#4010,#4011,#4012,#4013,#4014));
#1241=EDGE_LOOP('',(#4015,#4016,#4017,#4018,#4019,#4020));
#1242=EDGE_LOOP('',(#4021,#4022,#4023,#4024));
#1243=EDGE_LOOP('',(#4025));
#1244=EDGE_LOOP('',(#4026));
#1245=EDGE_LOOP('',(#4027,#4028,#4029,#4030,#4031,#4032));
#1246=EDGE_LOOP('',(#4033));
#1247=EDGE_LOOP('',(#4034,#4035,#4036,#4037,#4038,#4039));
#1248=EDGE_LOOP('',(#4040));
#1249=EDGE_LOOP('',(#4041,#4042,#4043,#4044));
#1250=EDGE_LOOP('',(#4045,#4046,#4047,#4048));
#1251=EDGE_LOOP('',(#4049,#4050,#4051,#4052));
#1252=EDGE_LOOP('',(#4053,#4054,#4055,#4056));
#1253=EDGE_LOOP('',(#4057,#4058,#4059,#4060));
#1254=EDGE_LOOP('',(#4061,#4062,#4063,#4064));
#1255=EDGE_LOOP('',(#4065));
#1256=EDGE_LOOP('',(#4066));
#1257=EDGE_LOOP('',(#4067,#4068,#4069,#4070));
#1258=EDGE_LOOP('',(#4071));
#1259=EDGE_LOOP('',(#4072));
#1260=EDGE_LOOP('',(#4073,#4074,#4075,#4076));
#1261=EDGE_LOOP('',(#4077,#4078,#4079,#4080));
#1262=EDGE_LOOP('',(#4081));
#1263=EDGE_LOOP('',(#4082));
#1264=EDGE_LOOP('',(#4083,#4084,#4085,#4086));
#1265=EDGE_LOOP('',(#4087));
#1266=EDGE_LOOP('',(#4088));
#1267=EDGE_LOOP('',(#4089,#4090,#4091,#4092));
#1268=EDGE_LOOP('',(#4093));
#1269=EDGE_LOOP('',(#4094));
#1270=EDGE_LOOP('',(#4095,#4096,#4097,#4098));
#1271=EDGE_LOOP('',(#4099));
#1272=EDGE_LOOP('',(#4100));
#1273=EDGE_LOOP('',(#4101,#4102,#4103,#4104));
#1274=EDGE_LOOP('',(#4105,#4106,#4107,#4108));
#1275=EDGE_LOOP('',(#4109,#4110,#4111,#4112));
#1276=EDGE_LOOP('',(#4113));
#1277=EDGE_LOOP('',(#4114));
#1278=EDGE_LOOP('',(#4115));
#1279=EDGE_LOOP('',(#4116));
#1280=EDGE_LOOP('',(#4117,#4118,#4119,#4120));
#1281=EDGE_LOOP('',(#4121,#4122,#4123,#4124));
#1282=EDGE_LOOP('',(#4125,#4126,#4127,#4128));
#1283=EDGE_LOOP('',(#4129));
#1284=EDGE_LOOP('',(#4130));
#1285=EDGE_LOOP('',(#4131));
#1286=EDGE_LOOP('',(#4132));
#1287=EDGE_LOOP('',(#4133,#4134,#4135,#4136));
#1288=EDGE_LOOP('',(#4137,#4138,#4139,#4140));
#1289=EDGE_LOOP('',(#4141));
#1290=EDGE_LOOP('',(#4142));
#1291=EDGE_LOOP('',(#4143,#4144,#4145,#4146));
#1292=EDGE_LOOP('',(#4147,#4148,#4149,#4150));
#1293=EDGE_LOOP('',(#4151));
#1294=EDGE_LOOP('',(#4152));
#1295=EDGE_LOOP('',(#4153,#4154,#4155,#4156));
#1296=EDGE_LOOP('',(#4157));
#1297=EDGE_LOOP('',(#4158));
#1298=EDGE_LOOP('',(#4159,#4160,#4161,#4162,#4163,#4164,#4165,#4166,#4167));
#1299=EDGE_LOOP('',(#4168,#4169,#4170,#4171,#4172,#4173,#4174,#4175,#4176));
#1300=EDGE_LOOP('',(#4177,#4178,#4179,#4180));
#1301=EDGE_LOOP('',(#4181,#4182,#4183,#4184));
#1302=EDGE_LOOP('',(#4185,#4186,#4187,#4188));
#1303=EDGE_LOOP('',(#4189,#4190,#4191,#4192));
#1304=EDGE_LOOP('',(#4193,#4194,#4195,#4196));
#1305=EDGE_LOOP('',(#4197,#4198,#4199,#4200));
#1306=EDGE_LOOP('',(#4201,#4202,#4203,#4204));
#1307=EDGE_LOOP('',(#4205));
#1308=EDGE_LOOP('',(#4206));
#1309=EDGE_LOOP('',(#4207));
#1310=EDGE_LOOP('',(#4208));
#1311=EDGE_LOOP('',(#4209,#4210,#4211,#4212));
#1312=EDGE_LOOP('',(#4213));
#1313=EDGE_LOOP('',(#4214));
#1314=EDGE_LOOP('',(#4215,#4216,#4217,#4218));
#1315=EDGE_LOOP('',(#4219));
#1316=EDGE_LOOP('',(#4220));
#1317=EDGE_LOOP('',(#4221));
#1318=EDGE_LOOP('',(#4222));
#1319=EDGE_LOOP('',(#4223,#4224,#4225,#4226));
#1320=EDGE_LOOP('',(#4227,#4228,#4229,#4230));
#1321=EDGE_LOOP('',(#4231,#4232,#4233,#4234));
#1322=EDGE_LOOP('',(#4235));
#1323=EDGE_LOOP('',(#4236));
#1324=EDGE_LOOP('',(#4237));
#1325=EDGE_LOOP('',(#4238));
#1326=EDGE_LOOP('',(#4239,#4240,#4241,#4242));
#1327=EDGE_LOOP('',(#4243,#4244,#4245,#4246));
#1328=EDGE_LOOP('',(#4247));
#1329=EDGE_LOOP('',(#4248,#4249,#4250,#4251));
#1330=EDGE_LOOP('',(#4252));
#1331=EDGE_LOOP('',(#4253));
#1332=EDGE_LOOP('',(#4254));
#1333=EDGE_LOOP('',(#4255));
#1334=EDGE_LOOP('',(#4256,#4257,#4258,#4259));
#1335=EDGE_LOOP('',(#4260,#4261,#4262,#4263));
#1336=EDGE_LOOP('',(#4264,#4265,#4266,#4267));
#1337=EDGE_LOOP('',(#4268));
#1338=EDGE_LOOP('',(#4269));
#1339=EDGE_LOOP('',(#4270,#4271,#4272,#4273));
#1340=EDGE_LOOP('',(#4274,#4275,#4276,#4277));
#1341=EDGE_LOOP('',(#4278,#4279,#4280,#4281));
#1342=EDGE_LOOP('',(#4282));
#1343=EDGE_LOOP('',(#4283,#4284,#4285,#4286));
#1344=EDGE_LOOP('',(#4287,#4288,#4289,#4290));
#1345=EDGE_LOOP('',(#4291,#4292,#4293,#4294));
#1346=EDGE_LOOP('',(#4295,#4296,#4297,#4298));
#1347=EDGE_LOOP('',(#4299,#4300,#4301,#4302));
#1348=EDGE_LOOP('',(#4303,#4304,#4305,#4306));
#1349=EDGE_LOOP('',(#4307,#4308,#4309,#4310,#4311,#4312));
#1350=EDGE_LOOP('',(#4313,#4314,#4315,#4316,#4317,#4318));
#1351=EDGE_LOOP('',(#4319,#4320,#4321,#4322));
#1352=EDGE_LOOP('',(#4323,#4324,#4325,#4326));
#1353=EDGE_LOOP('',(#4327,#4328));
#1354=EDGE_LOOP('',(#4329,#4330,#4331,#4332,#4333,#4334,#4335,#4336));
#1355=EDGE_LOOP('',(#4337,#4338,#4339));
#1356=EDGE_LOOP('',(#4340,#4341,#4342,#4343));
#1357=EDGE_LOOP('',(#4344,#4345,#4346,#4347));
#1358=EDGE_LOOP('',(#4348,#4349,#4350,#4351));
#1359=EDGE_LOOP('',(#4352));
#1360=EDGE_LOOP('',(#4353,#4354,#4355,#4356));
#1361=EDGE_LOOP('',(#4357));
#1362=EDGE_LOOP('',(#4358,#4359,#4360,#4361));
#1363=EDGE_LOOP('',(#4362));
#1364=EDGE_LOOP('',(#4363,#4364,#4365,#4366,#4367,#4368,#4369,#4370));
#1365=EDGE_LOOP('',(#4371,#4372,#4373,#4374));
#1366=EDGE_LOOP('',(#4375,#4376,#4377,#4378));
#1367=EDGE_LOOP('',(#4379,#4380,#4381,#4382));
#1368=EDGE_LOOP('',(#4383));
#1369=EDGE_LOOP('',(#4384,#4385,#4386,#4387));
#1370=EDGE_LOOP('',(#4388));
#1371=EDGE_LOOP('',(#4389,#4390,#4391,#4392));
#1372=EDGE_LOOP('',(#4393));
#1373=EDGE_LOOP('',(#4394,#4395,#4396,#4397,#4398,#4399,#4400,#4401));
#1374=EDGE_LOOP('',(#4402));
#1375=EDGE_LOOP('',(#4403,#4404,#4405,#4406));
#1376=EDGE_LOOP('',(#4407,#4408,#4409,#4410));
#1377=EDGE_LOOP('',(#4411,#4412,#4413,#4414));
#1378=EDGE_LOOP('',(#4415,#4416,#4417,#4418));
#1379=EDGE_LOOP('',(#4419,#4420,#4421,#4422));
#1380=EDGE_LOOP('',(#4423,#4424,#4425,#4426));
#1381=EDGE_LOOP('',(#4427,#4428,#4429,#4430,#4431,#4432));
#1382=EDGE_LOOP('',(#4433));
#1383=EDGE_LOOP('',(#4434,#4435,#4436,#4437,#4438,#4439));
#1384=EDGE_LOOP('',(#4440,#4441,#4442,#4443));
#1385=EDGE_LOOP('',(#4444,#4445,#4446,#4447));
#1386=EDGE_LOOP('',(#4448,#4449,#4450,#4451));
#1387=EDGE_LOOP('',(#4452));
#1388=EDGE_LOOP('',(#4453,#4454,#4455,#4456,#4457,#4458));
#1389=EDGE_LOOP('',(#4459));
#1390=EDGE_LOOP('',(#4460,#4461,#4462,#4463));
#1391=EDGE_LOOP('',(#4464,#4465,#4466,#4467));
#1392=EDGE_LOOP('',(#4468));
#1393=EDGE_LOOP('',(#4469));
#1394=EDGE_LOOP('',(#4470,#4471,#4472,#4473,#4474,#4475,#4476,#4477,#4478));
#1395=EDGE_LOOP('',(#4479));
#1396=EDGE_LOOP('',(#4480,#4481,#4482,#4483));
#1397=EDGE_LOOP('',(#4484));
#1398=EDGE_LOOP('',(#4485,#4486,#4487,#4488));
#1399=EDGE_LOOP('',(#4489,#4490,#4491,#4492));
#1400=EDGE_LOOP('',(#4493));
#1401=EDGE_LOOP('',(#4494));
#1402=EDGE_LOOP('',(#4495));
#1403=EDGE_LOOP('',(#4496));
#1404=EDGE_LOOP('',(#4497,#4498,#4499,#4500));
#1405=EDGE_LOOP('',(#4501,#4502));
#1406=EDGE_LOOP('',(#4503,#4504));
#1407=EDGE_LOOP('',(#4505,#4506,#4507,#4508));
#1408=EDGE_LOOP('',(#4509,#4510,#4511,#4512,#4513,#4514,#4515,#4516,#4517));
#1409=EDGE_LOOP('',(#4518,#4519,#4520));
#1410=LINE('',#7503,#1759);
#1411=LINE('',#7510,#1760);
#1412=LINE('',#7516,#1761);
#1413=LINE('',#7520,#1762);
#1414=LINE('',#7528,#1763);
#1415=LINE('',#7530,#1764);
#1416=LINE('',#7535,#1765);
#1417=LINE('',#7539,#1766);
#1418=LINE('',#7543,#1767);
#1419=LINE('',#7554,#1768);
#1420=LINE('',#7562,#1769);
#1421=LINE('',#7570,#1770);
#1422=LINE('',#7578,#1771);
#1423=LINE('',#7585,#1772);
#1424=LINE('',#7591,#1773);
#1425=LINE('',#7597,#1774);
#1426=LINE('',#7603,#1775);
#1427=LINE('',#7609,#1776);
#1428=LINE('',#7615,#1777);
#1429=LINE('',#7617,#1778);
#1430=LINE('',#7619,#1779);
#1431=LINE('',#7620,#1780);
#1432=LINE('',#7623,#1781);
#1433=LINE('',#7625,#1782);
#1434=LINE('',#7626,#1783);
#1435=LINE('',#7629,#1784);
#1436=LINE('',#7631,#1785);
#1437=LINE('',#7632,#1786);
#1438=LINE('',#7634,#1787);
#1439=LINE('',#7635,#1788);
#1440=LINE('',#7643,#1789);
#1441=LINE('',#7648,#1790);
#1442=LINE('',#7650,#1791);
#1443=LINE('',#7652,#1792);
#1444=LINE('',#7653,#1793);
#1445=LINE('',#7664,#1794);
#1446=LINE('',#7673,#1795);
#1447=LINE('',#7676,#1796);
#1448=LINE('',#7684,#1797);
#1449=LINE('',#7686,#1798);
#1450=LINE('',#7688,#1799);
#1451=LINE('',#7690,#1800);
#1452=LINE('',#7692,#1801);
#1453=LINE('',#7693,#1802);
#1454=LINE('',#7697,#1803);
#1455=LINE('',#7699,#1804);
#1456=LINE('',#7701,#1805);
#1457=LINE('',#7702,#1806);
#1458=LINE('',#7705,#1807);
#1459=LINE('',#7706,#1808);
#1460=LINE('',#7708,#1809);
#1461=LINE('',#7709,#1810);
#1462=LINE('',#7712,#1811);
#1463=LINE('',#7713,#1812);
#1464=LINE('',#7716,#1813);
#1465=LINE('',#7717,#1814);
#1466=LINE('',#7718,#1815);
#1467=LINE('',#7722,#1816);
#1468=LINE('',#7724,#1817);
#1469=LINE('',#7725,#1818);
#1470=LINE('',#7728,#1819);
#1471=LINE('',#7729,#1820);
#1472=LINE('',#7733,#1821);
#1473=LINE('',#7735,#1822);
#1474=LINE('',#7737,#1823);
#1475=LINE('',#7739,#1824);
#1476=LINE('',#7741,#1825);
#1477=LINE('',#7742,#1826);
#1478=LINE('',#7746,#1827);
#1479=LINE('',#7747,#1828);
#1480=LINE('',#7750,#1829);
#1481=LINE('',#7751,#1830);
#1482=LINE('',#7753,#1831);
#1483=LINE('',#7754,#1832);
#1484=LINE('',#7756,#1833);
#1485=LINE('',#7758,#1834);
#1486=LINE('',#7763,#1835);
#1487=LINE('',#7767,#1836);
#1488=LINE('',#7775,#1837);
#1489=LINE('',#7779,#1838);
#1490=LINE('',#7783,#1839);
#1491=LINE('',#7790,#1840);
#1492=LINE('',#7797,#1841);
#1493=LINE('',#7804,#1842);
#1494=LINE('',#7810,#1843);
#1495=LINE('',#7814,#1844);
#1496=LINE('',#7818,#1845);
#1497=LINE('',#7823,#1846);
#1498=LINE('',#7827,#1847);
#1499=LINE('',#7831,#1848);
#1500=LINE('',#7836,#1849);
#1501=LINE('',#7838,#1850);
#1502=LINE('',#7859,#1851);
#1503=LINE('',#7869,#1852);
#1504=LINE('',#7876,#1853);
#1505=LINE('',#7882,#1854);
#1506=LINE('',#7888,#1855);
#1507=LINE('',#7894,#1856);
#1508=LINE('',#7899,#1857);
#1509=LINE('',#7903,#1858);
#1510=LINE('',#7905,#1859);
#1511=LINE('',#7907,#1860);
#1512=LINE('',#7908,#1861);
#1513=LINE('',#7911,#1862);
#1514=LINE('',#7913,#1863);
#1515=LINE('',#7914,#1864);
#1516=LINE('',#7917,#1865);
#1517=LINE('',#7919,#1866);
#1518=LINE('',#7920,#1867);
#1519=LINE('',#7922,#1868);
#1520=LINE('',#7923,#1869);
#1521=LINE('',#7931,#1870);
#1522=LINE('',#7936,#1871);
#1523=LINE('',#7938,#1872);
#1524=LINE('',#7940,#1873);
#1525=LINE('',#7941,#1874);
#1526=LINE('',#7952,#1875);
#1527=LINE('',#7961,#1876);
#1528=LINE('',#7964,#1877);
#1529=LINE('',#7972,#1878);
#1530=LINE('',#7974,#1879);
#1531=LINE('',#7976,#1880);
#1532=LINE('',#7978,#1881);
#1533=LINE('',#7980,#1882);
#1534=LINE('',#7981,#1883);
#1535=LINE('',#7985,#1884);
#1536=LINE('',#7987,#1885);
#1537=LINE('',#7989,#1886);
#1538=LINE('',#7990,#1887);
#1539=LINE('',#7993,#1888);
#1540=LINE('',#7994,#1889);
#1541=LINE('',#7996,#1890);
#1542=LINE('',#7997,#1891);
#1543=LINE('',#8000,#1892);
#1544=LINE('',#8001,#1893);
#1545=LINE('',#8004,#1894);
#1546=LINE('',#8005,#1895);
#1547=LINE('',#8006,#1896);
#1548=LINE('',#8010,#1897);
#1549=LINE('',#8012,#1898);
#1550=LINE('',#8013,#1899);
#1551=LINE('',#8016,#1900);
#1552=LINE('',#8017,#1901);
#1553=LINE('',#8021,#1902);
#1554=LINE('',#8023,#1903);
#1555=LINE('',#8025,#1904);
#1556=LINE('',#8027,#1905);
#1557=LINE('',#8029,#1906);
#1558=LINE('',#8030,#1907);
#1559=LINE('',#8034,#1908);
#1560=LINE('',#8035,#1909);
#1561=LINE('',#8038,#1910);
#1562=LINE('',#8039,#1911);
#1563=LINE('',#8041,#1912);
#1564=LINE('',#8042,#1913);
#1565=LINE('',#8044,#1914);
#1566=LINE('',#8046,#1915);
#1567=LINE('',#8051,#1916);
#1568=LINE('',#8055,#1917);
#1569=LINE('',#8063,#1918);
#1570=LINE('',#8067,#1919);
#1571=LINE('',#8071,#1920);
#1572=LINE('',#8078,#1921);
#1573=LINE('',#8085,#1922);
#1574=LINE('',#8091,#1923);
#1575=LINE('',#8100,#1924);
#1576=LINE('',#8106,#1925);
#1577=LINE('',#8115,#1926);
#1578=LINE('',#8121,#1927);
#1579=LINE('',#8130,#1928);
#1580=LINE('',#8136,#1929);
#1581=LINE('',#8142,#1930);
#1582=LINE('',#8151,#1931);
#1583=LINE('',#8158,#1932);
#1584=LINE('',#8162,#1933);
#1585=LINE('',#8167,#1934);
#1586=LINE('',#8169,#1935);
#1587=LINE('',#8171,#1936);
#1588=LINE('',#8172,#1937);
#1589=LINE('',#8175,#1938);
#1590=LINE('',#8177,#1939);
#1591=LINE('',#8178,#1940);
#1592=LINE('',#8181,#1941);
#1593=LINE('',#8183,#1942);
#1594=LINE('',#8184,#1943);
#1595=LINE('',#8186,#1944);
#1596=LINE('',#8187,#1945);
#1597=LINE('',#8197,#1946);
#1598=LINE('',#8201,#1947);
#1599=LINE('',#8205,#1948);
#1600=LINE('',#8212,#1949);
#1601=LINE('',#8216,#1950);
#1602=LINE('',#8220,#1951);
#1603=LINE('',#8225,#1952);
#1604=LINE('',#8227,#1953);
#1605=LINE('',#8229,#1954);
#1606=LINE('',#8230,#1955);
#1607=LINE('',#8233,#1956);
#1608=LINE('',#8235,#1957);
#1609=LINE('',#8236,#1958);
#1610=LINE('',#8239,#1959);
#1611=LINE('',#8241,#1960);
#1612=LINE('',#8242,#1961);
#1613=LINE('',#8245,#1962);
#1614=LINE('',#8247,#1963);
#1615=LINE('',#8248,#1964);
#1616=LINE('',#8251,#1965);
#1617=LINE('',#8253,#1966);
#1618=LINE('',#8254,#1967);
#1619=LINE('',#8256,#1968);
#1620=LINE('',#8257,#1969);
#1621=LINE('',#8266,#1970);
#1622=LINE('',#8274,#1971);
#1623=LINE('',#8276,#1972);
#1624=LINE('',#8278,#1973);
#1625=LINE('',#8280,#1974);
#1626=LINE('',#8282,#1975);
#1627=LINE('',#8283,#1976);
#1628=LINE('',#8289,#1977);
#1629=LINE('',#8291,#1978);
#1630=LINE('',#8293,#1979);
#1631=LINE('',#8295,#1980);
#1632=LINE('',#8297,#1981);
#1633=LINE('',#8298,#1982);
#1634=LINE('',#8302,#1983);
#1635=LINE('',#8303,#1984);
#1636=LINE('',#8305,#1985);
#1637=LINE('',#8307,#1986);
#1638=LINE('',#8309,#1987);
#1639=LINE('',#8311,#1988);
#1640=LINE('',#8318,#1989);
#1641=LINE('',#8324,#1990);
#1642=LINE('',#8328,#1991);
#1643=LINE('',#8333,#1992);
#1644=LINE('',#8343,#1993);
#1645=LINE('',#8350,#1994);
#1646=LINE('',#8355,#1995);
#1647=LINE('',#8368,#1996);
#1648=LINE('',#8378,#1997);
#1649=LINE('',#8383,#1998);
#1650=LINE('',#8388,#1999);
#1651=LINE('',#8402,#2000);
#1652=LINE('',#8411,#2001);
#1653=LINE('',#8415,#2002);
#1654=LINE('',#8422,#2003);
#1655=LINE('',#8437,#2004);
#1656=LINE('',#8458,#2005);
#1657=LINE('',#8483,#2006);
#1658=LINE('',#8484,#2007);
#1659=LINE('',#8486,#2008);
#1660=LINE('',#8488,#2009);
#1661=LINE('',#8493,#2010);
#1662=LINE('',#8496,#2011);
#1663=LINE('',#8498,#2012);
#1664=LINE('',#8549,#2013);
#1665=LINE('',#8558,#2014);
#1666=LINE('',#8568,#2015);
#1667=LINE('',#8572,#2016);
#1668=LINE('',#8577,#2017);
#1669=LINE('',#8590,#2018);
#1670=LINE('',#8597,#2019);
#1671=LINE('',#8608,#2020);
#1672=LINE('',#8612,#2021);
#1673=LINE('',#8616,#2022);
#1674=LINE('',#8623,#2023);
#1675=LINE('',#8627,#2024);
#1676=LINE('',#8631,#2025);
#1677=LINE('',#8636,#2026);
#1678=LINE('',#8638,#2027);
#1679=LINE('',#8640,#2028);
#1680=LINE('',#8641,#2029);
#1681=LINE('',#8644,#2030);
#1682=LINE('',#8646,#2031);
#1683=LINE('',#8647,#2032);
#1684=LINE('',#8650,#2033);
#1685=LINE('',#8652,#2034);
#1686=LINE('',#8653,#2035);
#1687=LINE('',#8656,#2036);
#1688=LINE('',#8658,#2037);
#1689=LINE('',#8659,#2038);
#1690=LINE('',#8662,#2039);
#1691=LINE('',#8664,#2040);
#1692=LINE('',#8665,#2041);
#1693=LINE('',#8667,#2042);
#1694=LINE('',#8668,#2043);
#1695=LINE('',#8676,#2044);
#1696=LINE('',#8682,#2045);
#1697=LINE('',#8687,#2046);
#1698=LINE('',#8704,#2047);
#1699=LINE('',#8719,#2048);
#1700=LINE('',#8724,#2049);
#1701=LINE('',#8729,#2050);
#1702=LINE('',#8731,#2051);
#1703=LINE('',#8733,#2052);
#1704=LINE('',#8734,#2053);
#1705=LINE('',#8737,#2054);
#1706=LINE('',#8739,#2055);
#1707=LINE('',#8740,#2056);
#1708=LINE('',#8743,#2057);
#1709=LINE('',#8745,#2058);
#1710=LINE('',#8746,#2059);
#1711=LINE('',#8749,#2060);
#1712=LINE('',#8751,#2061);
#1713=LINE('',#8753,#2062);
#1714=LINE('',#8755,#2063);
#1715=LINE('',#8756,#2064);
#1716=LINE('',#8759,#2065);
#1717=LINE('',#8760,#2066);
#1718=LINE('',#8763,#2067);
#1719=LINE('',#8764,#2068);
#1720=LINE('',#8767,#2069);
#1721=LINE('',#8769,#2070);
#1722=LINE('',#8770,#2071);
#1723=LINE('',#8772,#2072);
#1724=LINE('',#8774,#2073);
#1725=LINE('',#8780,#2074);
#1726=LINE('',#8782,#2075);
#1727=LINE('',#8784,#2076);
#1728=LINE('',#8785,#2077);
#1729=LINE('',#8788,#2078);
#1730=LINE('',#8790,#2079);
#1731=LINE('',#8791,#2080);
#1732=LINE('',#8794,#2081);
#1733=LINE('',#8796,#2082);
#1734=LINE('',#8797,#2083);
#1735=LINE('',#8800,#2084);
#1736=LINE('',#8802,#2085);
#1737=LINE('',#8803,#2086);
#1738=LINE('',#8806,#2087);
#1739=LINE('',#8808,#2088);
#1740=LINE('',#8809,#2089);
#1741=LINE('',#8811,#2090);
#1742=LINE('',#8812,#2091);
#1743=LINE('',#8820,#2092);
#1744=LINE('',#8824,#2093);
#1745=LINE('',#8828,#2094);
#1746=LINE('',#8845,#2095);
#1747=LINE('',#8915,#2096);
#1748=LINE('',#8919,#2097);
#1749=LINE('',#8926,#2098);
#1750=LINE('',#8927,#2099);
#1751=LINE('',#8931,#2100);
#1752=LINE('',#8938,#2101);
#1753=LINE('',#8944,#2102);
#1754=LINE('',#9011,#2103);
#1755=LINE('',#9014,#2104);
#1756=LINE('',#9016,#2105);
#1757=LINE('',#9017,#2106);
#1758=LINE('',#9021,#2107);
#1759=VECTOR('',#5901,0.21);
#1760=VECTOR('',#5910,0.21);
#1761=VECTOR('',#5917,1.);
#1762=VECTOR('',#5922,1.);
#1763=VECTOR('',#5933,1.);
#1764=VECTOR('',#5934,1.);
#1765=VECTOR('',#5939,0.2);
#1766=VECTOR('',#5942,1.);
#1767=VECTOR('',#5945,1.);
#1768=VECTOR('',#5964,1.);
#1769=VECTOR('',#5977,0.2);
#1770=VECTOR('',#5988,1.);
#1771=VECTOR('',#5999,0.685);
#1772=VECTOR('',#6008,0.275);
#1773=VECTOR('',#6015,0.275);
#1774=VECTOR('',#6022,0.275);
#1775=VECTOR('',#6029,0.275);
#1776=VECTOR('',#6036,0.6);
#1777=VECTOR('',#6043,1.);
#1778=VECTOR('',#6044,1.);
#1779=VECTOR('',#6045,1.);
#1780=VECTOR('',#6046,1.);
#1781=VECTOR('',#6049,1.);
#1782=VECTOR('',#6050,1.);
#1783=VECTOR('',#6051,1.);
#1784=VECTOR('',#6054,1.);
#1785=VECTOR('',#6055,1.);
#1786=VECTOR('',#6056,1.);
#1787=VECTOR('',#6059,1.);
#1788=VECTOR('',#6060,1.);
#1789=VECTOR('',#6071,0.515);
#1790=VECTOR('',#6076,1.);
#1791=VECTOR('',#6077,1.);
#1792=VECTOR('',#6078,1.);
#1793=VECTOR('',#6079,1.);
#1794=VECTOR('',#6094,0.49);
#1795=VECTOR('',#6107,0.25);
#1796=VECTOR('',#6110,0.25);
#1797=VECTOR('',#6119,1.);
#1798=VECTOR('',#6120,1.);
#1799=VECTOR('',#6121,1.);
#1800=VECTOR('',#6122,1.);
#1801=VECTOR('',#6123,1.);
#1802=VECTOR('',#6124,1.);
#1803=VECTOR('',#6127,1.);
#1804=VECTOR('',#6128,1.);
#1805=VECTOR('',#6129,1.);
#1806=VECTOR('',#6130,1.);
#1807=VECTOR('',#6133,1.);
#1808=VECTOR('',#6134,1.);
#1809=VECTOR('',#6135,1.);
#1810=VECTOR('',#6136,1.);
#1811=VECTOR('',#6139,1.);
#1812=VECTOR('',#6140,1.);
#1813=VECTOR('',#6143,1.);
#1814=VECTOR('',#6144,1.);
#1815=VECTOR('',#6145,1.);
#1816=VECTOR('',#6150,1.);
#1817=VECTOR('',#6151,1.);
#1818=VECTOR('',#6152,1.);
#1819=VECTOR('',#6155,1.);
#1820=VECTOR('',#6156,1.);
#1821=VECTOR('',#6159,1.);
#1822=VECTOR('',#6160,1.);
#1823=VECTOR('',#6161,1.);
#1824=VECTOR('',#6162,1.);
#1825=VECTOR('',#6163,1.);
#1826=VECTOR('',#6164,1.);
#1827=VECTOR('',#6169,1.);
#1828=VECTOR('',#6170,1.);
#1829=VECTOR('',#6173,1.);
#1830=VECTOR('',#6174,1.);
#1831=VECTOR('',#6177,1.);
#1832=VECTOR('',#6178,1.);
#1833=VECTOR('',#6181,1.);
#1834=VECTOR('',#6184,1.);
#1835=VECTOR('',#6191,0.2);
#1836=VECTOR('',#6196,0.685);
#1837=VECTOR('',#6207,0.1);
#1838=VECTOR('',#6212,0.25);
#1839=VECTOR('',#6217,0.3);
#1840=VECTOR('',#6226,0.6);
#1841=VECTOR('',#6235,0.21);
#1842=VECTOR('',#6244,0.21);
#1843=VECTOR('',#6251,1.);
#1844=VECTOR('',#6256,1.);
#1845=VECTOR('',#6261,1.);
#1846=VECTOR('',#6266,1.);
#1847=VECTOR('',#6269,1.);
#1848=VECTOR('',#6272,0.2);
#1849=VECTOR('',#6277,1.);
#1850=VECTOR('',#6278,1.);
#1851=VECTOR('',#6317,0.2);
#1852=VECTOR('',#6330,0.685);
#1853=VECTOR('',#6339,0.275);
#1854=VECTOR('',#6346,0.275);
#1855=VECTOR('',#6353,0.275);
#1856=VECTOR('',#6360,0.275);
#1857=VECTOR('',#6367,1.);
#1858=VECTOR('',#6370,1.);
#1859=VECTOR('',#6371,1.);
#1860=VECTOR('',#6372,1.);
#1861=VECTOR('',#6373,1.);
#1862=VECTOR('',#6376,1.);
#1863=VECTOR('',#6377,1.);
#1864=VECTOR('',#6378,1.);
#1865=VECTOR('',#6381,1.);
#1866=VECTOR('',#6382,1.);
#1867=VECTOR('',#6383,1.);
#1868=VECTOR('',#6386,1.);
#1869=VECTOR('',#6387,1.);
#1870=VECTOR('',#6398,0.515);
#1871=VECTOR('',#6403,1.);
#1872=VECTOR('',#6404,1.);
#1873=VECTOR('',#6405,1.);
#1874=VECTOR('',#6406,1.);
#1875=VECTOR('',#6421,0.49);
#1876=VECTOR('',#6434,0.25);
#1877=VECTOR('',#6437,0.25);
#1878=VECTOR('',#6446,1.);
#1879=VECTOR('',#6447,1.);
#1880=VECTOR('',#6448,1.);
#1881=VECTOR('',#6449,1.);
#1882=VECTOR('',#6450,1.);
#1883=VECTOR('',#6451,1.);
#1884=VECTOR('',#6454,1.);
#1885=VECTOR('',#6455,1.);
#1886=VECTOR('',#6456,1.);
#1887=VECTOR('',#6457,1.);
#1888=VECTOR('',#6460,1.);
#1889=VECTOR('',#6461,1.);
#1890=VECTOR('',#6462,1.);
#1891=VECTOR('',#6463,1.);
#1892=VECTOR('',#6466,1.);
#1893=VECTOR('',#6467,1.);
#1894=VECTOR('',#6470,1.);
#1895=VECTOR('',#6471,1.);
#1896=VECTOR('',#6472,1.);
#1897=VECTOR('',#6477,1.);
#1898=VECTOR('',#6478,1.);
#1899=VECTOR('',#6479,1.);
#1900=VECTOR('',#6482,1.);
#1901=VECTOR('',#6483,1.);
#1902=VECTOR('',#6486,1.);
#1903=VECTOR('',#6487,1.);
#1904=VECTOR('',#6488,1.);
#1905=VECTOR('',#6489,1.);
#1906=VECTOR('',#6490,1.);
#1907=VECTOR('',#6491,1.);
#1908=VECTOR('',#6496,1.);
#1909=VECTOR('',#6497,1.);
#1910=VECTOR('',#6500,1.);
#1911=VECTOR('',#6501,1.);
#1912=VECTOR('',#6504,1.);
#1913=VECTOR('',#6505,1.);
#1914=VECTOR('',#6508,1.);
#1915=VECTOR('',#6511,1.);
#1916=VECTOR('',#6518,0.2);
#1917=VECTOR('',#6523,0.685);
#1918=VECTOR('',#6534,0.1);
#1919=VECTOR('',#6539,0.25);
#1920=VECTOR('',#6544,0.3);
#1921=VECTOR('',#6553,0.6);
#1922=VECTOR('',#6562,1.);
#1923=VECTOR('',#6569,1.6);
#1924=VECTOR('',#6582,1.);
#1925=VECTOR('',#6589,1.6);
#1926=VECTOR('',#6602,1.);
#1927=VECTOR('',#6609,1.6);
#1928=VECTOR('',#6622,0.275);
#1929=VECTOR('',#6629,0.275);
#1930=VECTOR('',#6636,0.5);
#1931=VECTOR('',#6647,0.5);
#1932=VECTOR('',#6656,0.275);
#1933=VECTOR('',#6661,0.275);
#1934=VECTOR('',#6666,1.);
#1935=VECTOR('',#6667,1.);
#1936=VECTOR('',#6668,1.);
#1937=VECTOR('',#6669,1.);
#1938=VECTOR('',#6672,1.);
#1939=VECTOR('',#6673,1.);
#1940=VECTOR('',#6674,1.);
#1941=VECTOR('',#6677,1.);
#1942=VECTOR('',#6678,1.);
#1943=VECTOR('',#6679,1.);
#1944=VECTOR('',#6682,1.);
#1945=VECTOR('',#6683,1.);
#1946=VECTOR('',#6698,0.4);
#1947=VECTOR('',#6703,0.425);
#1948=VECTOR('',#6708,0.41);
#1949=VECTOR('',#6717,0.26);
#1950=VECTOR('',#6722,0.25);
#1951=VECTOR('',#6727,0.225);
#1952=VECTOR('',#6732,1.);
#1953=VECTOR('',#6733,1.);
#1954=VECTOR('',#6734,1.);
#1955=VECTOR('',#6735,1.);
#1956=VECTOR('',#6738,1.);
#1957=VECTOR('',#6739,1.);
#1958=VECTOR('',#6740,1.);
#1959=VECTOR('',#6743,1.);
#1960=VECTOR('',#6744,1.);
#1961=VECTOR('',#6745,1.);
#1962=VECTOR('',#6748,1.);
#1963=VECTOR('',#6749,1.);
#1964=VECTOR('',#6750,1.);
#1965=VECTOR('',#6753,1.);
#1966=VECTOR('',#6754,1.);
#1967=VECTOR('',#6755,1.);
#1968=VECTOR('',#6758,1.);
#1969=VECTOR('',#6759,1.);
#1970=VECTOR('',#6772,0.43);
#1971=VECTOR('',#6781,1.);
#1972=VECTOR('',#6782,1.);
#1973=VECTOR('',#6783,1.);
#1974=VECTOR('',#6784,1.);
#1975=VECTOR('',#6785,1.);
#1976=VECTOR('',#6786,1.);
#1977=VECTOR('',#6791,1.);
#1978=VECTOR('',#6792,1.);
#1979=VECTOR('',#6793,1.);
#1980=VECTOR('',#6794,1.);
#1981=VECTOR('',#6795,1.);
#1982=VECTOR('',#6796,1.);
#1983=VECTOR('',#6801,1.);
#1984=VECTOR('',#6802,1.);
#1985=VECTOR('',#6805,1.);
#1986=VECTOR('',#6808,1.);
#1987=VECTOR('',#6811,1.);
#1988=VECTOR('',#6814,1.);
#1989=VECTOR('',#6823,0.46);
#1990=VECTOR('',#6832,0.525);
#1991=VECTOR('',#6837,0.515);
#1992=VECTOR('',#6844,0.2);
#1993=VECTOR('',#6857,0.475);
#1994=VECTOR('',#6866,0.355);
#1995=VECTOR('',#6873,0.31);
#1996=VECTOR('',#6892,0.51);
#1997=VECTOR('',#6905,0.405);
#1998=VECTOR('',#6912,0.405);
#1999=VECTOR('',#6917,0.6);
#2000=VECTOR('',#6938,0.25);
#2001=VECTOR('',#6951,0.275);
#2002=VECTOR('',#6956,0.265);
#2003=VECTOR('',#6965,0.5);
#2004=VECTOR('',#6974,0.47094010767585);
#2005=VECTOR('',#6981,0.47094010767585);
#2006=VECTOR('',#6984,1.);
#2007=VECTOR('',#6985,1.);
#2008=VECTOR('',#6988,1.);
#2009=VECTOR('',#6991,1.);
#2010=VECTOR('',#6996,0.25);
#2011=VECTOR('',#7001,1.);
#2012=VECTOR('',#7004,1.);
#2013=VECTOR('',#7101,0.4);
#2014=VECTOR('',#7112,0.9);
#2015=VECTOR('',#7125,0.99);
#2016=VECTOR('',#7130,0.225);
#2017=VECTOR('',#7137,0.99);
#2018=VECTOR('',#7156,0.165);
#2019=VECTOR('',#7165,0.4);
#2020=VECTOR('',#7182,0.325);
#2021=VECTOR('',#7187,0.35);
#2022=VECTOR('',#7192,0.335);
#2023=VECTOR('',#7201,0.21);
#2024=VECTOR('',#7206,0.2);
#2025=VECTOR('',#7211,0.18);
#2026=VECTOR('',#7216,1.);
#2027=VECTOR('',#7217,1.);
#2028=VECTOR('',#7218,1.);
#2029=VECTOR('',#7219,1.);
#2030=VECTOR('',#7222,1.);
#2031=VECTOR('',#7223,1.);
#2032=VECTOR('',#7224,1.);
#2033=VECTOR('',#7227,1.);
#2034=VECTOR('',#7228,1.);
#2035=VECTOR('',#7229,1.);
#2036=VECTOR('',#7232,1.);
#2037=VECTOR('',#7233,1.);
#2038=VECTOR('',#7234,1.);
#2039=VECTOR('',#7237,1.);
#2040=VECTOR('',#7238,1.);
#2041=VECTOR('',#7239,1.);
#2042=VECTOR('',#7242,1.);
#2043=VECTOR('',#7243,1.);
#2044=VECTOR('',#7254,0.305);
#2045=VECTOR('',#7261,0.305);
#2046=VECTOR('',#7266,1.);
#2047=VECTOR('',#7273,0.165);
#2048=VECTOR('',#7280,1.);
#2049=VECTOR('',#7285,0.4);
#2050=VECTOR('',#7290,1.);
#2051=VECTOR('',#7291,1.);
#2052=VECTOR('',#7292,1.);
#2053=VECTOR('',#7293,1.);
#2054=VECTOR('',#7296,1.);
#2055=VECTOR('',#7297,1.);
#2056=VECTOR('',#7298,1.);
#2057=VECTOR('',#7301,1.);
#2058=VECTOR('',#7302,1.);
#2059=VECTOR('',#7303,1.);
#2060=VECTOR('',#7306,1.);
#2061=VECTOR('',#7307,1.);
#2062=VECTOR('',#7308,1.);
#2063=VECTOR('',#7309,1.);
#2064=VECTOR('',#7310,1.);
#2065=VECTOR('',#7313,1.);
#2066=VECTOR('',#7314,1.);
#2067=VECTOR('',#7317,1.);
#2068=VECTOR('',#7318,1.);
#2069=VECTOR('',#7321,1.);
#2070=VECTOR('',#7322,1.);
#2071=VECTOR('',#7323,1.);
#2072=VECTOR('',#7326,1.);
#2073=VECTOR('',#7329,1.);
#2074=VECTOR('',#7336,1.);
#2075=VECTOR('',#7337,1.);
#2076=VECTOR('',#7338,1.);
#2077=VECTOR('',#7339,1.);
#2078=VECTOR('',#7342,1.);
#2079=VECTOR('',#7343,1.);
#2080=VECTOR('',#7344,1.);
#2081=VECTOR('',#7347,1.);
#2082=VECTOR('',#7348,1.);
#2083=VECTOR('',#7349,1.);
#2084=VECTOR('',#7352,1.);
#2085=VECTOR('',#7353,1.);
#2086=VECTOR('',#7354,1.);
#2087=VECTOR('',#7357,1.);
#2088=VECTOR('',#7358,1.);
#2089=VECTOR('',#7359,1.);
#2090=VECTOR('',#7362,1.);
#2091=VECTOR('',#7363,1.);
#2092=VECTOR('',#7374,0.185);
#2093=VECTOR('',#7379,0.2);
#2094=VECTOR('',#7384,0.1625);
#2095=VECTOR('',#7391,0.08);
#2096=VECTOR('',#7400,0.475);
#2097=VECTOR('',#7405,0.5);
#2098=VECTOR('',#7414,0.3);
#2099=VECTOR('',#7415,0.3);
#2100=VECTOR('',#7420,0.255);
#2101=VECTOR('',#7429,0.32);
#2102=VECTOR('',#7436,0.6);
#2103=VECTOR('',#7455,1.);
#2104=VECTOR('',#7458,1.);
#2105=VECTOR('',#7459,1.);
#2106=VECTOR('',#7460,1.);
#2107=VECTOR('',#7465,0.08);
#2108=CIRCLE('',#5267,0.21);
#2109=CIRCLE('',#5268,0.21);
#2110=CIRCLE('',#5271,0.21);
#2111=CIRCLE('',#5272,0.21);
#2112=CIRCLE('',#5275,0.2);
#2113=CIRCLE('',#5277,0.2);
#2114=CIRCLE('',#5284,0.2);
#2115=CIRCLE('',#5285,0.2);
#2116=CIRCLE('',#5286,0.2);
#2117=CIRCLE('',#5290,0.2);
#2118=CIRCLE('',#5293,1.);
#2119=CIRCLE('',#5296,0.2);
#2120=CIRCLE('',#5298,0.2);
#2121=CIRCLE('',#5301,0.2);
#2122=CIRCLE('',#5303,0.2);
#2123=CIRCLE('',#5305,1.);
#2124=CIRCLE('',#5306,1.);
#2125=CIRCLE('',#5307,1.);
#2126=CIRCLE('',#5310,0.685);
#2127=CIRCLE('',#5311,0.685);
#2128=CIRCLE('',#5314,0.275);
#2129=CIRCLE('',#5315,0.275);
#2130=CIRCLE('',#5317,0.275);
#2131=CIRCLE('',#5318,0.275);
#2132=CIRCLE('',#5320,0.275);
#2133=CIRCLE('',#5321,0.275);
#2134=CIRCLE('',#5323,0.275);
#2135=CIRCLE('',#5324,0.275);
#2136=CIRCLE('',#5326,0.6);
#2137=CIRCLE('',#5327,0.6);
#2138=CIRCLE('',#5337,0.515);
#2139=CIRCLE('',#5338,0.515);
#2140=CIRCLE('',#5341,0.4);
#2141=CIRCLE('',#5342,0.25);
#2142=CIRCLE('',#5344,0.4);
#2143=CIRCLE('',#5346,0.49);
#2144=CIRCLE('',#5347,0.49);
#2145=CIRCLE('',#5349,0.25);
#2146=CIRCLE('',#5351,0.25);
#2147=CIRCLE('',#5354,0.25);
#2148=CIRCLE('',#5356,0.2);
#2149=CIRCLE('',#5366,0.685);
#2150=CIRCLE('',#5375,0.2);
#2151=CIRCLE('',#5377,0.685);
#2152=CIRCLE('',#5381,0.2);
#2153=CIRCLE('',#5383,0.3);
#2154=CIRCLE('',#5385,0.3);
#2155=CIRCLE('',#5387,0.6);
#2156=CIRCLE('',#5389,0.6);
#2157=CIRCLE('',#5393,0.21);
#2158=CIRCLE('',#5394,0.21);
#2159=CIRCLE('',#5397,0.21);
#2160=CIRCLE('',#5398,0.21);
#2161=CIRCLE('',#5401,0.2);
#2162=CIRCLE('',#5403,0.2);
#2163=CIRCLE('',#5405,0.2);
#2164=CIRCLE('',#5407,0.2);
#2165=CIRCLE('',#5408,0.2);
#2166=CIRCLE('',#5412,0.2);
#2167=CIRCLE('',#5420,1.);
#2168=CIRCLE('',#5422,0.2);
#2169=CIRCLE('',#5424,0.2);
#2170=CIRCLE('',#5426,0.2);
#2171=CIRCLE('',#5430,0.2);
#2172=CIRCLE('',#5432,1.);
#2173=CIRCLE('',#5433,1.);
#2174=CIRCLE('',#5435,0.685);
#2175=CIRCLE('',#5436,0.685);
#2176=CIRCLE('',#5439,0.275);
#2177=CIRCLE('',#5440,0.275);
#2178=CIRCLE('',#5442,0.275);
#2179=CIRCLE('',#5443,0.275);
#2180=CIRCLE('',#5445,0.275);
#2181=CIRCLE('',#5446,0.275);
#2182=CIRCLE('',#5448,0.275);
#2183=CIRCLE('',#5449,0.275);
#2184=CIRCLE('',#5451,1.);
#2185=CIRCLE('',#5460,0.515);
#2186=CIRCLE('',#5461,0.515);
#2187=CIRCLE('',#5464,0.4);
#2188=CIRCLE('',#5465,0.25);
#2189=CIRCLE('',#5467,0.4);
#2190=CIRCLE('',#5469,0.49);
#2191=CIRCLE('',#5470,0.49);
#2192=CIRCLE('',#5472,0.25);
#2193=CIRCLE('',#5474,0.25);
#2194=CIRCLE('',#5477,0.25);
#2195=CIRCLE('',#5479,0.2);
#2196=CIRCLE('',#5489,0.685);
#2197=CIRCLE('',#5498,0.2);
#2198=CIRCLE('',#5500,0.685);
#2199=CIRCLE('',#5504,0.2);
#2200=CIRCLE('',#5506,0.3);
#2201=CIRCLE('',#5508,0.3);
#2202=CIRCLE('',#5510,0.6);
#2203=CIRCLE('',#5512,0.6);
#2204=CIRCLE('',#5516,1.);
#2205=CIRCLE('',#5517,1.);
#2206=CIRCLE('',#5519,1.6);
#2207=CIRCLE('',#5520,1.6);
#2208=CIRCLE('',#5525,1.);
#2209=CIRCLE('',#5526,1.);
#2210=CIRCLE('',#5528,1.6);
#2211=CIRCLE('',#5529,1.6);
#2212=CIRCLE('',#5534,1.);
#2213=CIRCLE('',#5535,1.);
#2214=CIRCLE('',#5537,1.6);
#2215=CIRCLE('',#5538,1.6);
#2216=CIRCLE('',#5543,0.275);
#2217=CIRCLE('',#5544,0.275);
#2218=CIRCLE('',#5546,0.275);
#2219=CIRCLE('',#5547,0.275);
#2220=CIRCLE('',#5549,0.5);
#2221=CIRCLE('',#5550,0.5);
#2222=CIRCLE('',#5552,0.275);
#2223=CIRCLE('',#5554,0.5);
#2224=CIRCLE('',#5555,0.5);
#2225=CIRCLE('',#5557,0.275);
#2226=CIRCLE('',#5559,0.275);
#2227=CIRCLE('',#5561,0.275);
#2228=CIRCLE('',#5570,0.375);
#2229=CIRCLE('',#5572,0.425);
#2230=CIRCLE('',#5574,0.425);
#2231=CIRCLE('',#5576,0.395);
#2232=CIRCLE('',#5578,0.27);
#2233=CIRCLE('',#5580,0.24505);
#2234=CIRCLE('',#5582,0.24505);
#2235=CIRCLE('',#5584,0.2);
#2236=CIRCLE('',#5597,0.43);
#2237=CIRCLE('',#5598,0.43);
#2238=CIRCLE('',#5600,0.2);
#2239=CIRCLE('',#5602,0.525);
#2240=CIRCLE('',#5604,0.515);
#2241=CIRCLE('',#5612,0.46);
#2242=CIRCLE('',#5614,0.46);
#2243=CIRCLE('',#5616,0.525);
#2244=CIRCLE('',#5619,0.515);
#2245=CIRCLE('',#5621,0.2);
#2246=CIRCLE('',#5625,0.475);
#2247=CIRCLE('',#5626,0.31);
#2248=CIRCLE('',#5628,0.475);
#2249=CIRCLE('',#5630,0.355);
#2250=CIRCLE('',#5632,0.355);
#2251=CIRCLE('',#5634,0.31);
#2252=CIRCLE('',#5640,0.089);
#2253=CIRCLE('',#5641,0.3035);
#2254=CIRCLE('',#5644,0.51);
#2255=CIRCLE('',#5645,0.51);
#2256=CIRCLE('',#5647,0.405);
#2257=CIRCLE('',#5649,0.405);
#2258=CIRCLE('',#5651,0.405);
#2259=CIRCLE('',#5653,0.405);
#2260=CIRCLE('',#5655,0.6);
#2261=CIRCLE('',#5656,0.6);
#2262=CIRCLE('',#5661,0.05);
#2263=CIRCLE('',#5662,0.4);
#2264=CIRCLE('',#5665,0.25);
#2265=CIRCLE('',#5666,0.25);
#2266=CIRCLE('',#5671,0.285);
#2267=CIRCLE('',#5672,0.265);
#2268=CIRCLE('',#5674,0.265);
#2269=CIRCLE('',#5676,0.5);
#2270=CIRCLE('',#5678,0.5);
#2271=CIRCLE('',#5682,0.38);
#2272=CIRCLE('',#5684,0.38);
#2273=CIRCLE('',#5689,0.2117);
#2274=CIRCLE('',#5690,0.2117);
#2275=CIRCLE('',#5740,0.4);
#2276=CIRCLE('',#5741,0.4);
#2277=CIRCLE('',#5743,0.225);
#2278=CIRCLE('',#5745,0.9);
#2279=CIRCLE('',#5746,0.9);
#2280=CIRCLE('',#5748,0.99);
#2281=CIRCLE('',#5750,0.99);
#2282=CIRCLE('',#5752,0.99);
#2283=CIRCLE('',#5754,0.225);
#2284=CIRCLE('',#5756,0.99);
#2285=CIRCLE('',#5761,0.05);
#2286=CIRCLE('',#5762,0.9);
#2287=CIRCLE('',#5765,0.165);
#2288=CIRCLE('',#5766,0.165);
#2289=CIRCLE('',#5769,0.4);
#2290=CIRCLE('',#5770,0.4);
#2291=CIRCLE('',#5775,0.3);
#2292=CIRCLE('',#5777,0.35);
#2293=CIRCLE('',#5779,0.35);
#2294=CIRCLE('',#5781,0.32);
#2295=CIRCLE('',#5783,0.22);
#2296=CIRCLE('',#5785,0.1954);
#2297=CIRCLE('',#5787,0.1954);
#2298=CIRCLE('',#5789,0.16);
#2299=CIRCLE('',#5801,0.305);
#2300=CIRCLE('',#5802,0.305);
#2301=CIRCLE('',#5804,0.305);
#2302=CIRCLE('',#5805,0.305);
#2303=CIRCLE('',#5807,0.165);
#2304=CIRCLE('',#5809,0.165);
#2305=CIRCLE('',#5810,0.165);
#2306=CIRCLE('',#5811,0.165);
#2307=CIRCLE('',#5814,0.4);
#2308=CIRCLE('',#5815,0.4);
#2309=CIRCLE('',#5835,0.17);
#2310=CIRCLE('',#5837,0.1954);
#2311=CIRCLE('',#5839,0.1954);
#2312=CIRCLE('',#5841,0.125);
#2313=CIRCLE('',#5846,0.45);
#2314=CIRCLE('',#5848,0.5);
#2315=CIRCLE('',#5850,0.5);
#2316=CIRCLE('',#5852,0.3);
#2317=CIRCLE('',#5854,0.3);
#2318=CIRCLE('',#5856,0.21);
#2319=CIRCLE('',#5860,0.32);
#2320=CIRCLE('',#5861,0.32);
#2321=CIRCLE('',#5863,0.6);
#2322=CIRCLE('',#5864,0.6);
#2323=CIRCLE('',#5869,0.08);
#2324=CIRCLE('',#5870,0.04);
#2325=CIRCLE('',#5872,0.08);
#2326=CIRCLE('',#5875,0.08);
#2327=CIRCLE('',#5876,0.08);
#2328=VERTEX_POINT('',#7500);
#2329=VERTEX_POINT('',#7502);
#2330=VERTEX_POINT('',#7507);
#2331=VERTEX_POINT('',#7509);
#2332=VERTEX_POINT('',#7514);
#2333=VERTEX_POINT('',#7515);
#2334=VERTEX_POINT('',#7519);
#2335=VERTEX_POINT('',#7523);
#2336=VERTEX_POINT('',#7527);
#2337=VERTEX_POINT('',#7529);
#2338=VERTEX_POINT('',#7532);
#2339=VERTEX_POINT('',#7534);
#2340=VERTEX_POINT('',#7536);
#2341=VERTEX_POINT('',#7538);
#2342=VERTEX_POINT('',#7540);
#2343=VERTEX_POINT('',#7542);
#2344=VERTEX_POINT('',#7547);
#2345=VERTEX_POINT('',#7561);
#2346=VERTEX_POINT('',#7567);
#2347=VERTEX_POINT('',#7569);
#2348=VERTEX_POINT('',#7575);
#2349=VERTEX_POINT('',#7577);
#2350=VERTEX_POINT('',#7582);
#2351=VERTEX_POINT('',#7584);
#2352=VERTEX_POINT('',#7588);
#2353=VERTEX_POINT('',#7590);
#2354=VERTEX_POINT('',#7594);
#2355=VERTEX_POINT('',#7596);
#2356=VERTEX_POINT('',#7600);
#2357=VERTEX_POINT('',#7602);
#2358=VERTEX_POINT('',#7606);
#2359=VERTEX_POINT('',#7608);
#2360=VERTEX_POINT('',#7613);
#2361=VERTEX_POINT('',#7614);
#2362=VERTEX_POINT('',#7616);
#2363=VERTEX_POINT('',#7618);
#2364=VERTEX_POINT('',#7622);
#2365=VERTEX_POINT('',#7624);
#2366=VERTEX_POINT('',#7628);
#2367=VERTEX_POINT('',#7630);
#2368=VERTEX_POINT('',#7640);
#2369=VERTEX_POINT('',#7642);
#2370=VERTEX_POINT('',#7646);
#2371=VERTEX_POINT('',#7647);
#2372=VERTEX_POINT('',#7649);
#2373=VERTEX_POINT('',#7651);
#2374=VERTEX_POINT('',#7656);
#2375=VERTEX_POINT('',#7661);
#2376=VERTEX_POINT('',#7663);
#2377=VERTEX_POINT('',#7667);
#2378=VERTEX_POINT('',#7670);
#2379=VERTEX_POINT('',#7675);
#2380=VERTEX_POINT('',#7679);
#2381=VERTEX_POINT('',#7682);
#2382=VERTEX_POINT('',#7683);
#2383=VERTEX_POINT('',#7685);
#2384=VERTEX_POINT('',#7687);
#2385=VERTEX_POINT('',#7689);
#2386=VERTEX_POINT('',#7691);
#2387=VERTEX_POINT('',#7695);
#2388=VERTEX_POINT('',#7696);
#2389=VERTEX_POINT('',#7698);
#2390=VERTEX_POINT('',#7700);
#2391=VERTEX_POINT('',#7704);
#2392=VERTEX_POINT('',#7707);
#2393=VERTEX_POINT('',#7711);
#2394=VERTEX_POINT('',#7715);
#2395=VERTEX_POINT('',#7721);
#2396=VERTEX_POINT('',#7723);
#2397=VERTEX_POINT('',#7727);
#2398=VERTEX_POINT('',#7731);
#2399=VERTEX_POINT('',#7732);
#2400=VERTEX_POINT('',#7734);
#2401=VERTEX_POINT('',#7736);
#2402=VERTEX_POINT('',#7738);
#2403=VERTEX_POINT('',#7740);
#2404=VERTEX_POINT('',#7743);
#2405=VERTEX_POINT('',#7749);
#2406=VERTEX_POINT('',#7762);
#2407=VERTEX_POINT('',#7766);
#2408=VERTEX_POINT('',#7772);
#2409=VERTEX_POINT('',#7774);
#2410=VERTEX_POINT('',#7777);
#2411=VERTEX_POINT('',#7781);
#2412=VERTEX_POINT('',#7785);
#2413=VERTEX_POINT('',#7788);
#2414=VERTEX_POINT('',#7794);
#2415=VERTEX_POINT('',#7796);
#2416=VERTEX_POINT('',#7801);
#2417=VERTEX_POINT('',#7803);
#2418=VERTEX_POINT('',#7808);
#2419=VERTEX_POINT('',#7809);
#2420=VERTEX_POINT('',#7813);
#2421=VERTEX_POINT('',#7817);
#2422=VERTEX_POINT('',#7821);
#2423=VERTEX_POINT('',#7822);
#2424=VERTEX_POINT('',#7824);
#2425=VERTEX_POINT('',#7826);
#2426=VERTEX_POINT('',#7828);
#2427=VERTEX_POINT('',#7830);
#2428=VERTEX_POINT('',#7832);
#2429=VERTEX_POINT('',#7834);
#2430=VERTEX_POINT('',#7837);
#2431=VERTEX_POINT('',#7858);
#2432=VERTEX_POINT('',#7862);
#2433=VERTEX_POINT('',#7866);
#2434=VERTEX_POINT('',#7868);
#2435=VERTEX_POINT('',#7873);
#2436=VERTEX_POINT('',#7875);
#2437=VERTEX_POINT('',#7879);
#2438=VERTEX_POINT('',#7881);
#2439=VERTEX_POINT('',#7885);
#2440=VERTEX_POINT('',#7887);
#2441=VERTEX_POINT('',#7891);
#2442=VERTEX_POINT('',#7893);
#2443=VERTEX_POINT('',#7897);
#2444=VERTEX_POINT('',#7901);
#2445=VERTEX_POINT('',#7902);
#2446=VERTEX_POINT('',#7904);
#2447=VERTEX_POINT('',#7906);
#2448=VERTEX_POINT('',#7910);
#2449=VERTEX_POINT('',#7912);
#2450=VERTEX_POINT('',#7916);
#2451=VERTEX_POINT('',#7918);
#2452=VERTEX_POINT('',#7928);
#2453=VERTEX_POINT('',#7930);
#2454=VERTEX_POINT('',#7934);
#2455=VERTEX_POINT('',#7935);
#2456=VERTEX_POINT('',#7937);
#2457=VERTEX_POINT('',#7939);
#2458=VERTEX_POINT('',#7944);
#2459=VERTEX_POINT('',#7949);
#2460=VERTEX_POINT('',#7951);
#2461=VERTEX_POINT('',#7955);
#2462=VERTEX_POINT('',#7958);
#2463=VERTEX_POINT('',#7963);
#2464=VERTEX_POINT('',#7967);
#2465=VERTEX_POINT('',#7970);
#2466=VERTEX_POINT('',#7971);
#2467=VERTEX_POINT('',#7973);
#2468=VERTEX_POINT('',#7975);
#2469=VERTEX_POINT('',#7977);
#2470=VERTEX_POINT('',#7979);
#2471=VERTEX_POINT('',#7983);
#2472=VERTEX_POINT('',#7984);
#2473=VERTEX_POINT('',#7986);
#2474=VERTEX_POINT('',#7988);
#2475=VERTEX_POINT('',#7992);
#2476=VERTEX_POINT('',#7995);
#2477=VERTEX_POINT('',#7999);
#2478=VERTEX_POINT('',#8003);
#2479=VERTEX_POINT('',#8009);
#2480=VERTEX_POINT('',#8011);
#2481=VERTEX_POINT('',#8015);
#2482=VERTEX_POINT('',#8019);
#2483=VERTEX_POINT('',#8020);
#2484=VERTEX_POINT('',#8022);
#2485=VERTEX_POINT('',#8024);
#2486=VERTEX_POINT('',#8026);
#2487=VERTEX_POINT('',#8028);
#2488=VERTEX_POINT('',#8031);
#2489=VERTEX_POINT('',#8037);
#2490=VERTEX_POINT('',#8050);
#2491=VERTEX_POINT('',#8054);
#2492=VERTEX_POINT('',#8060);
#2493=VERTEX_POINT('',#8062);
#2494=VERTEX_POINT('',#8065);
#2495=VERTEX_POINT('',#8069);
#2496=VERTEX_POINT('',#8073);
#2497=VERTEX_POINT('',#8076);
#2498=VERTEX_POINT('',#8082);
#2499=VERTEX_POINT('',#8084);
#2500=VERTEX_POINT('',#8088);
#2501=VERTEX_POINT('',#8090);
#2502=VERTEX_POINT('',#8097);
#2503=VERTEX_POINT('',#8099);
#2504=VERTEX_POINT('',#8103);
#2505=VERTEX_POINT('',#8105);
#2506=VERTEX_POINT('',#8112);
#2507=VERTEX_POINT('',#8114);
#2508=VERTEX_POINT('',#8118);
#2509=VERTEX_POINT('',#8120);
#2510=VERTEX_POINT('',#8127);
#2511=VERTEX_POINT('',#8129);
#2512=VERTEX_POINT('',#8133);
#2513=VERTEX_POINT('',#8135);
#2514=VERTEX_POINT('',#8139);
#2515=VERTEX_POINT('',#8141);
#2516=VERTEX_POINT('',#8145);
#2517=VERTEX_POINT('',#8148);
#2518=VERTEX_POINT('',#8150);
#2519=VERTEX_POINT('',#8154);
#2520=VERTEX_POINT('',#8157);
#2521=VERTEX_POINT('',#8161);
#2522=VERTEX_POINT('',#8165);
#2523=VERTEX_POINT('',#8166);
#2524=VERTEX_POINT('',#8168);
#2525=VERTEX_POINT('',#8170);
#2526=VERTEX_POINT('',#8174);
#2527=VERTEX_POINT('',#8176);
#2528=VERTEX_POINT('',#8180);
#2529=VERTEX_POINT('',#8182);
#2530=VERTEX_POINT('',#8192);
#2531=VERTEX_POINT('',#8195);
#2532=VERTEX_POINT('',#8199);
#2533=VERTEX_POINT('',#8203);
#2534=VERTEX_POINT('',#8207);
#2535=VERTEX_POINT('',#8210);
#2536=VERTEX_POINT('',#8214);
#2537=VERTEX_POINT('',#8218);
#2538=VERTEX_POINT('',#8223);
#2539=VERTEX_POINT('',#8224);
#2540=VERTEX_POINT('',#8226);
#2541=VERTEX_POINT('',#8228);
#2542=VERTEX_POINT('',#8232);
#2543=VERTEX_POINT('',#8234);
#2544=VERTEX_POINT('',#8238);
#2545=VERTEX_POINT('',#8240);
#2546=VERTEX_POINT('',#8244);
#2547=VERTEX_POINT('',#8246);
#2548=VERTEX_POINT('',#8250);
#2549=VERTEX_POINT('',#8252);
#2550=VERTEX_POINT('',#8263);
#2551=VERTEX_POINT('',#8265);
#2552=VERTEX_POINT('',#8269);
#2553=VERTEX_POINT('',#8272);
#2554=VERTEX_POINT('',#8273);
#2555=VERTEX_POINT('',#8275);
#2556=VERTEX_POINT('',#8277);
#2557=VERTEX_POINT('',#8279);
#2558=VERTEX_POINT('',#8281);
#2559=VERTEX_POINT('',#8284);
#2560=VERTEX_POINT('',#8287);
#2561=VERTEX_POINT('',#8288);
#2562=VERTEX_POINT('',#8290);
#2563=VERTEX_POINT('',#8292);
#2564=VERTEX_POINT('',#8294);
#2565=VERTEX_POINT('',#8296);
#2566=VERTEX_POINT('',#8299);
#2567=VERTEX_POINT('',#8314);
#2568=VERTEX_POINT('',#8317);
#2569=VERTEX_POINT('',#8321);
#2570=VERTEX_POINT('',#8326);
#2571=VERTEX_POINT('',#8330);
#2572=VERTEX_POINT('',#8336);
#2573=VERTEX_POINT('',#8338);
#2574=VERTEX_POINT('',#8341);
#2575=VERTEX_POINT('',#8345);
#2576=VERTEX_POINT('',#8348);
#2577=VERTEX_POINT('',#8352);
#2578=VERTEX_POINT('',#8360);
#2579=VERTEX_POINT('',#8365);
#2580=VERTEX_POINT('',#8367);
#2581=VERTEX_POINT('',#8371);
#2582=VERTEX_POINT('',#8374);
#2583=VERTEX_POINT('',#8377);
#2584=VERTEX_POINT('',#8381);
#2585=VERTEX_POINT('',#8385);
#2586=VERTEX_POINT('',#8387);
#2587=VERTEX_POINT('',#8394);
#2588=VERTEX_POINT('',#8399);
#2589=VERTEX_POINT('',#8401);
#2590=VERTEX_POINT('',#8408);
#2591=VERTEX_POINT('',#8410);
#2592=VERTEX_POINT('',#8414);
#2593=VERTEX_POINT('',#8418);
#2594=VERTEX_POINT('',#8421);
#2595=VERTEX_POINT('',#8427);
#2596=VERTEX_POINT('',#8428);
#2597=VERTEX_POINT('',#8432);
#2598=VERTEX_POINT('',#8436);
#2599=VERTEX_POINT('',#8439);
#2600=VERTEX_POINT('',#8443);
#2601=VERTEX_POINT('',#8447);
#2602=VERTEX_POINT('',#8455);
#2603=VERTEX_POINT('',#8457);
#2604=VERTEX_POINT('',#8459);
#2605=VERTEX_POINT('',#8463);
#2606=VERTEX_POINT('',#8467);
#2607=VERTEX_POINT('',#8471);
#2608=VERTEX_POINT('',#8475);
#2609=VERTEX_POINT('',#8490);
#2610=VERTEX_POINT('',#8492);
#2611=VERTEX_POINT('',#8546);
#2612=VERTEX_POINT('',#8548);
#2613=VERTEX_POINT('',#8552);
#2614=VERTEX_POINT('',#8555);
#2615=VERTEX_POINT('',#8557);
#2616=VERTEX_POINT('',#8561);
#2617=VERTEX_POINT('',#8564);
#2618=VERTEX_POINT('',#8567);
#2619=VERTEX_POINT('',#8571);
#2620=VERTEX_POINT('',#8575);
#2621=VERTEX_POINT('',#8582);
#2622=VERTEX_POINT('',#8587);
#2623=VERTEX_POINT('',#8589);
#2624=VERTEX_POINT('',#8594);
#2625=VERTEX_POINT('',#8596);
#2626=VERTEX_POINT('',#8603);
#2627=VERTEX_POINT('',#8606);
#2628=VERTEX_POINT('',#8610);
#2629=VERTEX_POINT('',#8614);
#2630=VERTEX_POINT('',#8618);
#2631=VERTEX_POINT('',#8621);
#2632=VERTEX_POINT('',#8625);
#2633=VERTEX_POINT('',#8629);
#2634=VERTEX_POINT('',#8634);
#2635=VERTEX_POINT('',#8635);
#2636=VERTEX_POINT('',#8637);
#2637=VERTEX_POINT('',#8639);
#2638=VERTEX_POINT('',#8643);
#2639=VERTEX_POINT('',#8645);
#2640=VERTEX_POINT('',#8649);
#2641=VERTEX_POINT('',#8651);
#2642=VERTEX_POINT('',#8655);
#2643=VERTEX_POINT('',#8657);
#2644=VERTEX_POINT('',#8661);
#2645=VERTEX_POINT('',#8663);
#2646=VERTEX_POINT('',#8673);
#2647=VERTEX_POINT('',#8675);
#2648=VERTEX_POINT('',#8679);
#2649=VERTEX_POINT('',#8681);
#2650=VERTEX_POINT('',#8685);
#2651=VERTEX_POINT('',#8686);
#2652=VERTEX_POINT('',#8690);
#2653=VERTEX_POINT('',#8701);
#2654=VERTEX_POINT('',#8703);
#2655=VERTEX_POINT('',#8706);
#2656=VERTEX_POINT('',#8721);
#2657=VERTEX_POINT('',#8723);
#2658=VERTEX_POINT('',#8727);
#2659=VERTEX_POINT('',#8728);
#2660=VERTEX_POINT('',#8730);
#2661=VERTEX_POINT('',#8732);
#2662=VERTEX_POINT('',#8736);
#2663=VERTEX_POINT('',#8738);
#2664=VERTEX_POINT('',#8742);
#2665=VERTEX_POINT('',#8744);
#2666=VERTEX_POINT('',#8748);
#2667=VERTEX_POINT('',#8750);
#2668=VERTEX_POINT('',#8752);
#2669=VERTEX_POINT('',#8754);
#2670=VERTEX_POINT('',#8758);
#2671=VERTEX_POINT('',#8762);
#2672=VERTEX_POINT('',#8766);
#2673=VERTEX_POINT('',#8768);
#2674=VERTEX_POINT('',#8778);
#2675=VERTEX_POINT('',#8779);
#2676=VERTEX_POINT('',#8781);
#2677=VERTEX_POINT('',#8783);
#2678=VERTEX_POINT('',#8787);
#2679=VERTEX_POINT('',#8789);
#2680=VERTEX_POINT('',#8793);
#2681=VERTEX_POINT('',#8795);
#2682=VERTEX_POINT('',#8799);
#2683=VERTEX_POINT('',#8801);
#2684=VERTEX_POINT('',#8805);
#2685=VERTEX_POINT('',#8807);
#2686=VERTEX_POINT('',#8815);
#2687=VERTEX_POINT('',#8818);
#2688=VERTEX_POINT('',#8822);
#2689=VERTEX_POINT('',#8826);
#2690=VERTEX_POINT('',#8832);
#2691=VERTEX_POINT('',#8833);
#2692=VERTEX_POINT('',#8844);
#2693=VERTEX_POINT('',#8880);
#2694=VERTEX_POINT('',#8910);
#2695=VERTEX_POINT('',#8913);
#2696=VERTEX_POINT('',#8917);
#2697=VERTEX_POINT('',#8921);
#2698=VERTEX_POINT('',#8924);
#2699=VERTEX_POINT('',#8929);
#2700=VERTEX_POINT('',#8935);
#2701=VERTEX_POINT('',#8937);
#2702=VERTEX_POINT('',#8941);
#2703=VERTEX_POINT('',#8943);
#2704=VERTEX_POINT('',#8950);
#2705=VERTEX_POINT('',#8953);
#2706=VERTEX_POINT('',#8954);
#2707=VERTEX_POINT('',#9008);
#2708=VERTEX_POINT('',#9009);
#2709=VERTEX_POINT('',#9013);
#2710=VERTEX_POINT('',#9015);
#2711=VERTEX_POINT('',#9019);
#2712=EDGE_CURVE('',#2328,#2328,#2108,.T.);
#2713=EDGE_CURVE('',#2328,#2329,#1410,.T.);
#2714=EDGE_CURVE('',#2329,#2329,#2109,.T.);
#2715=EDGE_CURVE('',#2330,#2330,#2110,.T.);
#2716=EDGE_CURVE('',#2330,#2331,#1411,.T.);
#2717=EDGE_CURVE('',#2331,#2331,#2111,.T.);
#2718=EDGE_CURVE('',#2332,#2333,#1412,.T.);
#2719=EDGE_CURVE('',#2332,#2333,#2112,.T.);
#2720=EDGE_CURVE('',#2334,#2332,#1413,.T.);
#2721=EDGE_CURVE('',#2334,#2332,#2113,.T.);
#2722=EDGE_CURVE('',#2335,#2334,#495,.T.);
#2723=EDGE_CURVE('',#2332,#2335,#496,.T.);
#2724=EDGE_CURVE('',#2333,#2336,#1414,.T.);
#2725=EDGE_CURVE('',#2337,#2332,#1415,.T.);
#2726=EDGE_CURVE('',#2335,#2337,#497,.T.);
#2727=EDGE_CURVE('',#2338,#2335,#498,.T.);
#2728=EDGE_CURVE('',#2338,#2339,#1416,.T.);
#2729=EDGE_CURVE('',#2340,#2339,#2114,.T.);
#2730=EDGE_CURVE('',#2341,#2340,#1417,.T.);
#2731=EDGE_CURVE('',#2341,#2342,#2115,.T.);
#2732=EDGE_CURVE('',#2343,#2342,#1418,.T.);
#2733=EDGE_CURVE('',#2339,#2343,#2116,.T.);
#2734=EDGE_CURVE('',#2336,#2338,#499,.T.);
#2735=EDGE_CURVE('',#2344,#2338,#500,.T.);
#2736=EDGE_CURVE('',#2333,#2344,#2117,.T.);
#2737=EDGE_CURVE('',#2338,#2333,#501,.T.);
#2738=EDGE_CURVE('',#2342,#2341,#2118,.T.);
#2739=EDGE_CURVE('',#2333,#2344,#1419,.T.);
#2740=EDGE_CURVE('',#2332,#2337,#2119,.T.);
#2741=EDGE_CURVE('',#2333,#2332,#2120,.T.);
#2742=EDGE_CURVE('',#2338,#2345,#1420,.T.);
#2743=EDGE_CURVE('',#2345,#2345,#2121,.T.);
#2744=EDGE_CURVE('',#2336,#2333,#2122,.T.);
#2745=EDGE_CURVE('',#2346,#2340,#2123,.T.);
#2746=EDGE_CURVE('',#2346,#2347,#1421,.T.);
#2747=EDGE_CURVE('',#2347,#2347,#2124,.T.);
#2748=EDGE_CURVE('',#2343,#2346,#2125,.T.);
#2749=EDGE_CURVE('',#2348,#2348,#2126,.T.);
#2750=EDGE_CURVE('',#2348,#2349,#1422,.T.);
#2751=EDGE_CURVE('',#2349,#2349,#2127,.T.);
#2752=EDGE_CURVE('',#2350,#2350,#2128,.T.);
#2753=EDGE_CURVE('',#2350,#2351,#1423,.T.);
#2754=EDGE_CURVE('',#2351,#2351,#2129,.T.);
#2755=EDGE_CURVE('',#2352,#2352,#2130,.T.);
#2756=EDGE_CURVE('',#2352,#2353,#1424,.T.);
#2757=EDGE_CURVE('',#2353,#2353,#2131,.T.);
#2758=EDGE_CURVE('',#2354,#2354,#2132,.T.);
#2759=EDGE_CURVE('',#2354,#2355,#1425,.T.);
#2760=EDGE_CURVE('',#2355,#2355,#2133,.T.);
#2761=EDGE_CURVE('',#2356,#2356,#2134,.T.);
#2762=EDGE_CURVE('',#2356,#2357,#1426,.T.);
#2763=EDGE_CURVE('',#2357,#2357,#2135,.T.);
#2764=EDGE_CURVE('',#2358,#2358,#2136,.T.);
#2765=EDGE_CURVE('',#2358,#2359,#1427,.T.);
#2766=EDGE_CURVE('',#2359,#2359,#2137,.T.);
#2767=EDGE_CURVE('',#2360,#2361,#1428,.T.);
#2768=EDGE_CURVE('',#2361,#2362,#1429,.T.);
#2769=EDGE_CURVE('',#2363,#2362,#1430,.T.);
#2770=EDGE_CURVE('',#2360,#2363,#1431,.T.);
#2771=EDGE_CURVE('',#2364,#2360,#1432,.T.);
#2772=EDGE_CURVE('',#2365,#2363,#1433,.T.);
#2773=EDGE_CURVE('',#2364,#2365,#1434,.T.);
#2774=EDGE_CURVE('',#2366,#2364,#1435,.T.);
#2775=EDGE_CURVE('',#2367,#2365,#1436,.T.);
#2776=EDGE_CURVE('',#2366,#2367,#1437,.T.);
#2777=EDGE_CURVE('',#2361,#2366,#1438,.T.);
#2778=EDGE_CURVE('',#2362,#2367,#1439,.T.);
#2779=EDGE_CURVE('',#2368,#2368,#2138,.T.);
#2780=EDGE_CURVE('',#2368,#2369,#1440,.T.);
#2781=EDGE_CURVE('',#2369,#2369,#2139,.T.);
#2782=EDGE_CURVE('',#2370,#2371,#1441,.T.);
#2783=EDGE_CURVE('',#2372,#2370,#1442,.T.);
#2784=EDGE_CURVE('',#2373,#2372,#1443,.T.);
#2785=EDGE_CURVE('',#2371,#2373,#1444,.T.);
#2786=EDGE_CURVE('',#2372,#2370,#2140,.T.);
#2787=EDGE_CURVE('',#2374,#2374,#2141,.T.);
#2788=EDGE_CURVE('',#2373,#2371,#2142,.T.);
#2789=EDGE_CURVE('',#2375,#2375,#2143,.T.);
#2790=EDGE_CURVE('',#2375,#2376,#1445,.T.);
#2791=EDGE_CURVE('',#2376,#2376,#2144,.T.);
#2792=EDGE_CURVE('',#2377,#2377,#2145,.T.);
#2793=EDGE_CURVE('',#2378,#2378,#2146,.T.);
#2794=EDGE_CURVE('',#2374,#2378,#1446,.T.);
#2795=EDGE_CURVE('',#2377,#2379,#1447,.T.);
#2796=EDGE_CURVE('',#2379,#2379,#2147,.T.);
#2797=EDGE_CURVE('',#2380,#2380,#2148,.T.);
#2798=EDGE_CURVE('',#2381,#2382,#1448,.T.);
#2799=EDGE_CURVE('',#2382,#2383,#1449,.T.);
#2800=EDGE_CURVE('',#2383,#2384,#1450,.T.);
#2801=EDGE_CURVE('',#2385,#2384,#1451,.T.);
#2802=EDGE_CURVE('',#2386,#2385,#1452,.T.);
#2803=EDGE_CURVE('',#2381,#2386,#1453,.T.);
#2804=EDGE_CURVE('',#2387,#2388,#1454,.T.);
#2805=EDGE_CURVE('',#2388,#2389,#1455,.T.);
#2806=EDGE_CURVE('',#2390,#2389,#1456,.T.);
#2807=EDGE_CURVE('',#2387,#2390,#1457,.T.);
#2808=EDGE_CURVE('',#2391,#2384,#1458,.T.);
#2809=EDGE_CURVE('',#2391,#2387,#1459,.T.);
#2810=EDGE_CURVE('',#2392,#2390,#1460,.T.);
#2811=EDGE_CURVE('',#2385,#2392,#1461,.T.);
#2812=EDGE_CURVE('',#2393,#2392,#1462,.T.);
#2813=EDGE_CURVE('',#2386,#2393,#1463,.T.);
#2814=EDGE_CURVE('',#2388,#2394,#1464,.T.);
#2815=EDGE_CURVE('',#2381,#2394,#1465,.T.);
#2816=EDGE_CURVE('',#2389,#2393,#1466,.T.);
#2817=EDGE_CURVE('',#2395,#2394,#1467,.T.);
#2818=EDGE_CURVE('',#2391,#2396,#1468,.T.);
#2819=EDGE_CURVE('',#2396,#2395,#1469,.T.);
#2820=EDGE_CURVE('',#2384,#2397,#1470,.T.);
#2821=EDGE_CURVE('',#2397,#2391,#1471,.T.);
#2822=EDGE_CURVE('',#2398,#2399,#1472,.T.);
#2823=EDGE_CURVE('',#2400,#2398,#1473,.T.);
#2824=EDGE_CURVE('',#2401,#2400,#1474,.T.);
#2825=EDGE_CURVE('',#2402,#2401,#1475,.T.);
#2826=EDGE_CURVE('',#2403,#2402,#1476,.T.);
#2827=EDGE_CURVE('',#2399,#2403,#1477,.T.);
#2828=EDGE_CURVE('',#2404,#2404,#2149,.T.);
#2829=EDGE_CURVE('',#2398,#2383,#1478,.T.);
#2830=EDGE_CURVE('',#2400,#2382,#1479,.T.);
#2831=EDGE_CURVE('',#2405,#2381,#1480,.T.);
#2832=EDGE_CURVE('',#2401,#2405,#1481,.T.);
#2833=EDGE_CURVE('',#2394,#2405,#1482,.T.);
#2834=EDGE_CURVE('',#2402,#2395,#1483,.T.);
#2835=EDGE_CURVE('',#2403,#2396,#1484,.T.);
#2836=EDGE_CURVE('',#2399,#2397,#1485,.T.);
#2837=EDGE_CURVE('',#2380,#2406,#1486,.T.);
#2838=EDGE_CURVE('',#2406,#2406,#2150,.T.);
#2839=EDGE_CURVE('',#2404,#2407,#1487,.T.);
#2840=EDGE_CURVE('',#2407,#2407,#2151,.T.);
#2841=EDGE_CURVE('',#2408,#2408,#2152,.T.);
#2842=EDGE_CURVE('',#2408,#2409,#1488,.T.);
#2843=EDGE_CURVE('',#2410,#2410,#2153,.T.);
#2844=EDGE_CURVE('',#2410,#2408,#1489,.T.);
#2845=EDGE_CURVE('',#2411,#2411,#2154,.T.);
#2846=EDGE_CURVE('',#2411,#2410,#1490,.T.);
#2847=EDGE_CURVE('',#2412,#2412,#2155,.T.);
#2848=EDGE_CURVE('',#2413,#2413,#2156,.T.);
#2849=EDGE_CURVE('',#2413,#2412,#1491,.T.);
#2850=EDGE_CURVE('',#2414,#2414,#2157,.T.);
#2851=EDGE_CURVE('',#2414,#2415,#1492,.T.);
#2852=EDGE_CURVE('',#2415,#2415,#2158,.T.);
#2853=EDGE_CURVE('',#2416,#2416,#2159,.T.);
#2854=EDGE_CURVE('',#2416,#2417,#1493,.T.);
#2855=EDGE_CURVE('',#2417,#2417,#2160,.T.);
#2856=EDGE_CURVE('',#2418,#2419,#1494,.T.);
#2857=EDGE_CURVE('',#2419,#2418,#2161,.T.);
#2858=EDGE_CURVE('',#2419,#2420,#1495,.T.);
#2859=EDGE_CURVE('',#2420,#2419,#2162,.T.);
#2860=EDGE_CURVE('',#2421,#2418,#1496,.T.);
#2861=EDGE_CURVE('',#2418,#2421,#2163,.T.);
#2862=EDGE_CURVE('',#2422,#2423,#1497,.T.);
#2863=EDGE_CURVE('',#2424,#2422,#2164,.T.);
#2864=EDGE_CURVE('',#2425,#2424,#1498,.T.);
#2865=EDGE_CURVE('',#2426,#2425,#2165,.T.);
#2866=EDGE_CURVE('',#2426,#2427,#1499,.T.);
#2867=EDGE_CURVE('',#2428,#2427,#502,.T.);
#2868=EDGE_CURVE('',#2429,#2428,#503,.T.);
#2869=EDGE_CURVE('',#2419,#2429,#1500,.T.);
#2870=EDGE_CURVE('',#2430,#2418,#1501,.T.);
#2871=EDGE_CURVE('',#2427,#2430,#504,.T.);
#2872=EDGE_CURVE('',#2423,#2426,#2166,.T.);
#2873=EDGE_CURVE('',#2420,#2428,#505,.T.);
#2874=EDGE_CURVE('',#2428,#2419,#506,.T.);
#2875=EDGE_CURVE('',#2427,#2421,#507,.T.);
#2876=EDGE_CURVE('',#2418,#2427,#508,.T.);
#2877=EDGE_CURVE('',#2424,#2422,#2167,.T.);
#2878=EDGE_CURVE('',#2419,#2418,#2168,.T.);
#2879=EDGE_CURVE('',#2429,#2419,#2169,.T.);
#2880=EDGE_CURVE('',#2418,#2430,#2170,.T.);
#2881=EDGE_CURVE('',#2427,#2431,#1502,.T.);
#2882=EDGE_CURVE('',#2431,#2431,#2171,.T.);
#2883=EDGE_CURVE('',#2432,#2425,#2172,.T.);
#2884=EDGE_CURVE('',#2423,#2432,#2173,.T.);
#2885=EDGE_CURVE('',#2433,#2433,#2174,.T.);
#2886=EDGE_CURVE('',#2433,#2434,#1503,.T.);
#2887=EDGE_CURVE('',#2434,#2434,#2175,.T.);
#2888=EDGE_CURVE('',#2435,#2435,#2176,.T.);
#2889=EDGE_CURVE('',#2435,#2436,#1504,.T.);
#2890=EDGE_CURVE('',#2436,#2436,#2177,.T.);
#2891=EDGE_CURVE('',#2437,#2437,#2178,.T.);
#2892=EDGE_CURVE('',#2437,#2438,#1505,.T.);
#2893=EDGE_CURVE('',#2438,#2438,#2179,.T.);
#2894=EDGE_CURVE('',#2439,#2439,#2180,.T.);
#2895=EDGE_CURVE('',#2439,#2440,#1506,.T.);
#2896=EDGE_CURVE('',#2440,#2440,#2181,.T.);
#2897=EDGE_CURVE('',#2441,#2441,#2182,.T.);
#2898=EDGE_CURVE('',#2441,#2442,#1507,.T.);
#2899=EDGE_CURVE('',#2442,#2442,#2183,.T.);
#2900=EDGE_CURVE('',#2443,#2443,#2184,.T.);
#2901=EDGE_CURVE('',#2443,#2432,#1508,.T.);
#2902=EDGE_CURVE('',#2444,#2445,#1509,.T.);
#2903=EDGE_CURVE('',#2445,#2446,#1510,.T.);
#2904=EDGE_CURVE('',#2447,#2446,#1511,.T.);
#2905=EDGE_CURVE('',#2444,#2447,#1512,.T.);
#2906=EDGE_CURVE('',#2448,#2444,#1513,.T.);
#2907=EDGE_CURVE('',#2449,#2447,#1514,.T.);
#2908=EDGE_CURVE('',#2448,#2449,#1515,.T.);
#2909=EDGE_CURVE('',#2450,#2448,#1516,.T.);
#2910=EDGE_CURVE('',#2451,#2449,#1517,.T.);
#2911=EDGE_CURVE('',#2450,#2451,#1518,.T.);
#2912=EDGE_CURVE('',#2445,#2450,#1519,.T.);
#2913=EDGE_CURVE('',#2446,#2451,#1520,.T.);
#2914=EDGE_CURVE('',#2452,#2452,#2185,.T.);
#2915=EDGE_CURVE('',#2452,#2453,#1521,.T.);
#2916=EDGE_CURVE('',#2453,#2453,#2186,.T.);
#2917=EDGE_CURVE('',#2454,#2455,#1522,.T.);
#2918=EDGE_CURVE('',#2456,#2454,#1523,.T.);
#2919=EDGE_CURVE('',#2457,#2456,#1524,.T.);
#2920=EDGE_CURVE('',#2455,#2457,#1525,.T.);
#2921=EDGE_CURVE('',#2456,#2454,#2187,.T.);
#2922=EDGE_CURVE('',#2458,#2458,#2188,.T.);
#2923=EDGE_CURVE('',#2457,#2455,#2189,.T.);
#2924=EDGE_CURVE('',#2459,#2459,#2190,.T.);
#2925=EDGE_CURVE('',#2459,#2460,#1526,.T.);
#2926=EDGE_CURVE('',#2460,#2460,#2191,.T.);
#2927=EDGE_CURVE('',#2461,#2461,#2192,.T.);
#2928=EDGE_CURVE('',#2462,#2462,#2193,.T.);
#2929=EDGE_CURVE('',#2458,#2462,#1527,.T.);
#2930=EDGE_CURVE('',#2461,#2463,#1528,.T.);
#2931=EDGE_CURVE('',#2463,#2463,#2194,.T.);
#2932=EDGE_CURVE('',#2464,#2464,#2195,.T.);
#2933=EDGE_CURVE('',#2465,#2466,#1529,.T.);
#2934=EDGE_CURVE('',#2466,#2467,#1530,.T.);
#2935=EDGE_CURVE('',#2467,#2468,#1531,.T.);
#2936=EDGE_CURVE('',#2469,#2468,#1532,.T.);
#2937=EDGE_CURVE('',#2470,#2469,#1533,.T.);
#2938=EDGE_CURVE('',#2465,#2470,#1534,.T.);
#2939=EDGE_CURVE('',#2471,#2472,#1535,.T.);
#2940=EDGE_CURVE('',#2472,#2473,#1536,.T.);
#2941=EDGE_CURVE('',#2474,#2473,#1537,.T.);
#2942=EDGE_CURVE('',#2471,#2474,#1538,.T.);
#2943=EDGE_CURVE('',#2475,#2468,#1539,.T.);
#2944=EDGE_CURVE('',#2475,#2471,#1540,.T.);
#2945=EDGE_CURVE('',#2476,#2474,#1541,.T.);
#2946=EDGE_CURVE('',#2469,#2476,#1542,.T.);
#2947=EDGE_CURVE('',#2477,#2476,#1543,.T.);
#2948=EDGE_CURVE('',#2470,#2477,#1544,.T.);
#2949=EDGE_CURVE('',#2472,#2478,#1545,.T.);
#2950=EDGE_CURVE('',#2465,#2478,#1546,.T.);
#2951=EDGE_CURVE('',#2473,#2477,#1547,.T.);
#2952=EDGE_CURVE('',#2479,#2478,#1548,.T.);
#2953=EDGE_CURVE('',#2475,#2480,#1549,.T.);
#2954=EDGE_CURVE('',#2480,#2479,#1550,.T.);
#2955=EDGE_CURVE('',#2468,#2481,#1551,.T.);
#2956=EDGE_CURVE('',#2481,#2475,#1552,.T.);
#2957=EDGE_CURVE('',#2482,#2483,#1553,.T.);
#2958=EDGE_CURVE('',#2484,#2482,#1554,.T.);
#2959=EDGE_CURVE('',#2485,#2484,#1555,.T.);
#2960=EDGE_CURVE('',#2486,#2485,#1556,.T.);
#2961=EDGE_CURVE('',#2487,#2486,#1557,.T.);
#2962=EDGE_CURVE('',#2483,#2487,#1558,.T.);
#2963=EDGE_CURVE('',#2488,#2488,#2196,.T.);
#2964=EDGE_CURVE('',#2482,#2467,#1559,.T.);
#2965=EDGE_CURVE('',#2484,#2466,#1560,.T.);
#2966=EDGE_CURVE('',#2489,#2465,#1561,.T.);
#2967=EDGE_CURVE('',#2485,#2489,#1562,.T.);
#2968=EDGE_CURVE('',#2478,#2489,#1563,.T.);
#2969=EDGE_CURVE('',#2486,#2479,#1564,.T.);
#2970=EDGE_CURVE('',#2487,#2480,#1565,.T.);
#2971=EDGE_CURVE('',#2483,#2481,#1566,.T.);
#2972=EDGE_CURVE('',#2464,#2490,#1567,.T.);
#2973=EDGE_CURVE('',#2490,#2490,#2197,.T.);
#2974=EDGE_CURVE('',#2488,#2491,#1568,.T.);
#2975=EDGE_CURVE('',#2491,#2491,#2198,.T.);
#2976=EDGE_CURVE('',#2492,#2492,#2199,.T.);
#2977=EDGE_CURVE('',#2492,#2493,#1569,.T.);
#2978=EDGE_CURVE('',#2494,#2494,#2200,.T.);
#2979=EDGE_CURVE('',#2494,#2492,#1570,.T.);
#2980=EDGE_CURVE('',#2495,#2495,#2201,.T.);
#2981=EDGE_CURVE('',#2495,#2494,#1571,.T.);
#2982=EDGE_CURVE('',#2496,#2496,#2202,.T.);
#2983=EDGE_CURVE('',#2497,#2497,#2203,.T.);
#2984=EDGE_CURVE('',#2497,#2496,#1572,.T.);
#2985=EDGE_CURVE('',#2498,#2498,#2204,.T.);
#2986=EDGE_CURVE('',#2498,#2499,#1573,.T.);
#2987=EDGE_CURVE('',#2499,#2499,#2205,.T.);
#2988=EDGE_CURVE('',#2500,#2500,#2206,.T.);
#2989=EDGE_CURVE('',#2500,#2501,#1574,.T.);
#2990=EDGE_CURVE('',#2501,#2501,#2207,.T.);
#2991=EDGE_CURVE('',#2502,#2502,#2208,.T.);
#2992=EDGE_CURVE('',#2502,#2503,#1575,.T.);
#2993=EDGE_CURVE('',#2503,#2503,#2209,.T.);
#2994=EDGE_CURVE('',#2504,#2504,#2210,.T.);
#2995=EDGE_CURVE('',#2504,#2505,#1576,.T.);
#2996=EDGE_CURVE('',#2505,#2505,#2211,.T.);
#2997=EDGE_CURVE('',#2506,#2506,#2212,.T.);
#2998=EDGE_CURVE('',#2506,#2507,#1577,.T.);
#2999=EDGE_CURVE('',#2507,#2507,#2213,.T.);
#3000=EDGE_CURVE('',#2508,#2508,#2214,.T.);
#3001=EDGE_CURVE('',#2508,#2509,#1578,.T.);
#3002=EDGE_CURVE('',#2509,#2509,#2215,.T.);
#3003=EDGE_CURVE('',#2510,#2510,#2216,.T.);
#3004=EDGE_CURVE('',#2510,#2511,#1579,.T.);
#3005=EDGE_CURVE('',#2511,#2511,#2217,.T.);
#3006=EDGE_CURVE('',#2512,#2512,#2218,.T.);
#3007=EDGE_CURVE('',#2512,#2513,#1580,.T.);
#3008=EDGE_CURVE('',#2513,#2513,#2219,.T.);
#3009=EDGE_CURVE('',#2514,#2514,#2220,.T.);
#3010=EDGE_CURVE('',#2514,#2515,#1581,.T.);
#3011=EDGE_CURVE('',#2515,#2515,#2221,.T.);
#3012=EDGE_CURVE('',#2516,#2516,#2222,.T.);
#3013=EDGE_CURVE('',#2517,#2517,#2223,.T.);
#3014=EDGE_CURVE('',#2517,#2518,#1582,.T.);
#3015=EDGE_CURVE('',#2518,#2518,#2224,.T.);
#3016=EDGE_CURVE('',#2519,#2519,#2225,.T.);
#3017=EDGE_CURVE('',#2516,#2520,#1583,.T.);
#3018=EDGE_CURVE('',#2520,#2520,#2226,.T.);
#3019=EDGE_CURVE('',#2519,#2521,#1584,.T.);
#3020=EDGE_CURVE('',#2521,#2521,#2227,.T.);
#3021=EDGE_CURVE('',#2522,#2523,#1585,.T.);
#3022=EDGE_CURVE('',#2523,#2524,#1586,.T.);
#3023=EDGE_CURVE('',#2525,#2524,#1587,.T.);
#3024=EDGE_CURVE('',#2522,#2525,#1588,.T.);
#3025=EDGE_CURVE('',#2526,#2522,#1589,.T.);
#3026=EDGE_CURVE('',#2527,#2525,#1590,.T.);
#3027=EDGE_CURVE('',#2526,#2527,#1591,.T.);
#3028=EDGE_CURVE('',#2528,#2526,#1592,.T.);
#3029=EDGE_CURVE('',#2529,#2527,#1593,.T.);
#3030=EDGE_CURVE('',#2528,#2529,#1594,.T.);
#3031=EDGE_CURVE('',#2523,#2528,#1595,.T.);
#3032=EDGE_CURVE('',#2524,#2529,#1596,.T.);
#3033=EDGE_CURVE('',#2530,#2530,#2228,.T.);
#3034=EDGE_CURVE('',#2531,#2531,#2229,.T.);
#3035=EDGE_CURVE('',#2531,#2530,#1597,.T.);
#3036=EDGE_CURVE('',#2532,#2532,#2230,.T.);
#3037=EDGE_CURVE('',#2532,#2531,#1598,.T.);
#3038=EDGE_CURVE('',#2533,#2533,#2231,.T.);
#3039=EDGE_CURVE('',#2533,#2532,#1599,.T.);
#3040=EDGE_CURVE('',#2534,#2534,#2232,.T.);
#3041=EDGE_CURVE('',#2535,#2535,#2233,.F.);
#3042=EDGE_CURVE('',#2535,#2534,#1600,.T.);
#3043=EDGE_CURVE('',#2536,#2536,#2234,.F.);
#3044=EDGE_CURVE('',#2536,#2535,#1601,.T.);
#3045=EDGE_CURVE('',#2537,#2537,#2235,.T.);
#3046=EDGE_CURVE('',#2537,#2536,#1602,.T.);
#3047=EDGE_CURVE('',#2538,#2539,#1603,.T.);
#3048=EDGE_CURVE('',#2539,#2540,#1604,.T.);
#3049=EDGE_CURVE('',#2540,#2541,#1605,.T.);
#3050=EDGE_CURVE('',#2538,#2541,#1606,.T.);
#3051=EDGE_CURVE('',#2539,#2542,#1607,.T.);
#3052=EDGE_CURVE('',#2542,#2543,#1608,.T.);
#3053=EDGE_CURVE('',#2543,#2540,#1609,.T.);
#3054=EDGE_CURVE('',#2542,#2544,#1610,.T.);
#3055=EDGE_CURVE('',#2544,#2545,#1611,.T.);
#3056=EDGE_CURVE('',#2545,#2543,#1612,.T.);
#3057=EDGE_CURVE('',#2544,#2546,#1613,.T.);
#3058=EDGE_CURVE('',#2546,#2547,#1614,.T.);
#3059=EDGE_CURVE('',#2547,#2545,#1615,.T.);
#3060=EDGE_CURVE('',#2546,#2548,#1616,.T.);
#3061=EDGE_CURVE('',#2548,#2549,#1617,.T.);
#3062=EDGE_CURVE('',#2549,#2547,#1618,.T.);
#3063=EDGE_CURVE('',#2548,#2538,#1619,.T.);
#3064=EDGE_CURVE('',#2541,#2549,#1620,.T.);
#3065=EDGE_CURVE('',#2550,#2550,#2236,.T.);
#3066=EDGE_CURVE('',#2550,#2551,#1621,.T.);
#3067=EDGE_CURVE('',#2551,#2551,#2237,.T.);
#3068=EDGE_CURVE('',#2552,#2552,#2238,.T.);
#3069=EDGE_CURVE('',#2553,#2554,#1622,.T.);
#3070=EDGE_CURVE('',#2554,#2555,#1623,.T.);
#3071=EDGE_CURVE('',#2555,#2556,#1624,.T.);
#3072=EDGE_CURVE('',#2556,#2557,#1625,.T.);
#3073=EDGE_CURVE('',#2557,#2558,#1626,.T.);
#3074=EDGE_CURVE('',#2558,#2553,#1627,.T.);
#3075=EDGE_CURVE('',#2559,#2559,#2239,.T.);
#3076=EDGE_CURVE('',#2560,#2561,#1628,.T.);
#3077=EDGE_CURVE('',#2562,#2560,#1629,.T.);
#3078=EDGE_CURVE('',#2563,#2562,#1630,.T.);
#3079=EDGE_CURVE('',#2564,#2563,#1631,.T.);
#3080=EDGE_CURVE('',#2565,#2564,#1632,.T.);
#3081=EDGE_CURVE('',#2561,#2565,#1633,.T.);
#3082=EDGE_CURVE('',#2566,#2566,#2240,.T.);
#3083=EDGE_CURVE('',#2560,#2553,#1634,.T.);
#3084=EDGE_CURVE('',#2562,#2558,#1635,.T.);
#3085=EDGE_CURVE('',#2563,#2557,#1636,.T.);
#3086=EDGE_CURVE('',#2564,#2556,#1637,.T.);
#3087=EDGE_CURVE('',#2565,#2555,#1638,.T.);
#3088=EDGE_CURVE('',#2561,#2554,#1639,.T.);
#3089=EDGE_CURVE('',#2567,#2567,#2241,.T.);
#3090=EDGE_CURVE('',#2567,#2568,#1640,.T.);
#3091=EDGE_CURVE('',#2568,#2568,#2242,.T.);
#3092=EDGE_CURVE('',#2569,#2569,#2243,.T.);
#3093=EDGE_CURVE('',#2559,#2569,#1641,.T.);
#3094=EDGE_CURVE('',#2570,#2570,#2244,.T.);
#3095=EDGE_CURVE('',#2570,#2566,#1642,.T.);
#3096=EDGE_CURVE('',#2571,#2571,#2245,.T.);
#3097=EDGE_CURVE('',#2571,#2552,#1643,.T.);
#3098=EDGE_CURVE('',#2572,#2572,#2246,.T.);
#3099=EDGE_CURVE('',#2573,#2573,#2247,.T.);
#3100=EDGE_CURVE('',#2574,#2574,#2248,.T.);
#3101=EDGE_CURVE('',#2574,#2572,#1644,.T.);
#3102=EDGE_CURVE('',#2575,#2575,#2249,.T.);
#3103=EDGE_CURVE('',#2576,#2576,#2250,.T.);
#3104=EDGE_CURVE('',#2576,#2575,#1645,.T.);
#3105=EDGE_CURVE('',#2577,#2577,#2251,.T.);
#3106=EDGE_CURVE('',#2577,#2573,#1646,.T.);
#3107=EDGE_CURVE('',#2578,#2578,#2252,.T.);
#3108=EDGE_CURVE('',#2578,#2578,#2253,.T.);
#3109=EDGE_CURVE('',#2579,#2579,#2254,.T.);
#3110=EDGE_CURVE('',#2579,#2580,#1647,.T.);
#3111=EDGE_CURVE('',#2580,#2580,#2255,.T.);
#3112=EDGE_CURVE('',#2581,#2581,#2256,.T.);
#3113=EDGE_CURVE('',#2582,#2582,#2257,.T.);
#3114=EDGE_CURVE('',#2582,#2583,#1648,.T.);
#3115=EDGE_CURVE('',#2583,#2583,#2258,.T.);
#3116=EDGE_CURVE('',#2584,#2584,#2259,.T.);
#3117=EDGE_CURVE('',#2584,#2581,#1649,.T.);
#3118=EDGE_CURVE('',#2585,#2585,#2260,.T.);
#3119=EDGE_CURVE('',#2585,#2586,#1650,.T.);
#3120=EDGE_CURVE('',#2586,#2586,#2261,.T.);
#3121=EDGE_CURVE('',#2587,#2587,#2262,.T.);
#3122=EDGE_CURVE('',#2587,#2587,#2263,.T.);
#3123=EDGE_CURVE('',#2588,#2588,#2264,.T.);
#3124=EDGE_CURVE('',#2588,#2589,#1651,.T.);
#3125=EDGE_CURVE('',#2589,#2589,#2265,.T.);
#3126=EDGE_CURVE('',#2590,#2590,#2266,.T.);
#3127=EDGE_CURVE('',#2590,#2591,#1652,.T.);
#3128=EDGE_CURVE('',#2591,#2591,#2267,.T.);
#3129=EDGE_CURVE('',#2591,#2592,#1653,.T.);
#3130=EDGE_CURVE('',#2592,#2592,#2268,.T.);
#3131=EDGE_CURVE('',#2593,#2593,#2269,.T.);
#3132=EDGE_CURVE('',#2593,#2594,#1654,.T.);
#3133=EDGE_CURVE('',#2594,#2594,#2270,.T.);
#3134=EDGE_CURVE('',#2595,#2596,#19,.T.);
#3135=EDGE_CURVE('',#2597,#2595,#20,.T.);
#3136=EDGE_CURVE('',#2597,#2598,#1655,.T.);
#3137=EDGE_CURVE('',#2598,#2598,#2271,.T.);
#3138=EDGE_CURVE('',#2599,#2597,#21,.T.);
#3139=EDGE_CURVE('',#2600,#2599,#22,.T.);
#3140=EDGE_CURVE('',#2601,#2600,#23,.T.);
#3141=EDGE_CURVE('',#2596,#2601,#24,.T.);
#3142=EDGE_CURVE('',#2602,#2602,#2272,.T.);
#3143=EDGE_CURVE('',#2602,#2603,#1656,.T.);
#3144=EDGE_CURVE('',#2604,#2603,#25,.T.);
#3145=EDGE_CURVE('',#2605,#2604,#26,.T.);
#3146=EDGE_CURVE('',#2606,#2605,#27,.T.);
#3147=EDGE_CURVE('',#2607,#2606,#28,.T.);
#3148=EDGE_CURVE('',#2608,#2607,#29,.T.);
#3149=EDGE_CURVE('',#2603,#2608,#30,.T.);
#3150=EDGE_CURVE('',#2599,#2608,#1657,.T.);
#3151=EDGE_CURVE('',#2600,#2607,#1658,.T.);
#3152=EDGE_CURVE('',#2597,#2603,#1659,.T.);
#3153=EDGE_CURVE('',#2595,#2604,#1660,.T.);
#3154=EDGE_CURVE('',#2609,#2609,#2273,.F.);
#3155=EDGE_CURVE('',#2609,#2610,#1661,.T.);
#3156=EDGE_CURVE('',#2610,#2610,#2274,.F.);
#3157=EDGE_CURVE('',#2596,#2605,#1662,.T.);
#3158=EDGE_CURVE('',#2601,#2606,#1663,.T.);
#3159=EDGE_CURVE('',#2611,#2611,#2275,.T.);
#3160=EDGE_CURVE('',#2611,#2612,#1664,.T.);
#3161=EDGE_CURVE('',#2612,#2612,#2276,.T.);
#3162=EDGE_CURVE('',#2613,#2613,#2277,.T.);
#3163=EDGE_CURVE('',#2614,#2614,#2278,.T.);
#3164=EDGE_CURVE('',#2614,#2615,#1665,.T.);
#3165=EDGE_CURVE('',#2615,#2615,#2279,.T.);
#3166=EDGE_CURVE('',#2616,#2616,#2280,.T.);
#3167=EDGE_CURVE('',#2617,#2617,#2281,.T.);
#3168=EDGE_CURVE('',#2617,#2618,#1666,.T.);
#3169=EDGE_CURVE('',#2618,#2618,#2282,.T.);
#3170=EDGE_CURVE('',#2613,#2619,#1667,.T.);
#3171=EDGE_CURVE('',#2619,#2619,#2283,.T.);
#3172=EDGE_CURVE('',#2620,#2620,#2284,.T.);
#3173=EDGE_CURVE('',#2620,#2616,#1668,.T.);
#3174=EDGE_CURVE('',#2621,#2621,#2285,.T.);
#3175=EDGE_CURVE('',#2621,#2621,#2286,.T.);
#3176=EDGE_CURVE('',#2622,#2622,#2287,.T.);
#3177=EDGE_CURVE('',#2622,#2623,#1669,.T.);
#3178=EDGE_CURVE('',#2623,#2623,#2288,.T.);
#3179=EDGE_CURVE('',#2624,#2624,#2289,.T.);
#3180=EDGE_CURVE('',#2624,#2625,#1670,.T.);
#3181=EDGE_CURVE('',#2625,#2625,#2290,.T.);
#3182=EDGE_CURVE('',#2626,#2626,#2291,.T.);
#3183=EDGE_CURVE('',#2627,#2627,#2292,.T.);
#3184=EDGE_CURVE('',#2627,#2626,#1671,.T.);
#3185=EDGE_CURVE('',#2628,#2628,#2293,.T.);
#3186=EDGE_CURVE('',#2628,#2627,#1672,.T.);
#3187=EDGE_CURVE('',#2629,#2629,#2294,.T.);
#3188=EDGE_CURVE('',#2629,#2628,#1673,.T.);
#3189=EDGE_CURVE('',#2630,#2630,#2295,.T.);
#3190=EDGE_CURVE('',#2631,#2631,#2296,.F.);
#3191=EDGE_CURVE('',#2631,#2630,#1674,.T.);
#3192=EDGE_CURVE('',#2632,#2632,#2297,.F.);
#3193=EDGE_CURVE('',#2632,#2631,#1675,.T.);
#3194=EDGE_CURVE('',#2633,#2633,#2298,.T.);
#3195=EDGE_CURVE('',#2633,#2632,#1676,.T.);
#3196=EDGE_CURVE('',#2634,#2635,#1677,.T.);
#3197=EDGE_CURVE('',#2635,#2636,#1678,.T.);
#3198=EDGE_CURVE('',#2636,#2637,#1679,.T.);
#3199=EDGE_CURVE('',#2634,#2637,#1680,.T.);
#3200=EDGE_CURVE('',#2635,#2638,#1681,.T.);
#3201=EDGE_CURVE('',#2638,#2639,#1682,.T.);
#3202=EDGE_CURVE('',#2639,#2636,#1683,.T.);
#3203=EDGE_CURVE('',#2638,#2640,#1684,.T.);
#3204=EDGE_CURVE('',#2640,#2641,#1685,.T.);
#3205=EDGE_CURVE('',#2641,#2639,#1686,.T.);
#3206=EDGE_CURVE('',#2640,#2642,#1687,.T.);
#3207=EDGE_CURVE('',#2642,#2643,#1688,.T.);
#3208=EDGE_CURVE('',#2643,#2641,#1689,.T.);
#3209=EDGE_CURVE('',#2642,#2644,#1690,.T.);
#3210=EDGE_CURVE('',#2644,#2645,#1691,.T.);
#3211=EDGE_CURVE('',#2645,#2643,#1692,.T.);
#3212=EDGE_CURVE('',#2644,#2634,#1693,.T.);
#3213=EDGE_CURVE('',#2637,#2645,#1694,.T.);
#3214=EDGE_CURVE('',#2646,#2646,#2299,.T.);
#3215=EDGE_CURVE('',#2646,#2647,#1695,.T.);
#3216=EDGE_CURVE('',#2647,#2647,#2300,.T.);
#3217=EDGE_CURVE('',#2648,#2648,#2301,.T.);
#3218=EDGE_CURVE('',#2648,#2649,#1696,.T.);
#3219=EDGE_CURVE('',#2649,#2649,#2302,.T.);
#3220=EDGE_CURVE('',#2650,#2651,#1697,.T.);
#3221=EDGE_CURVE('',#2650,#2651,#2303,.T.);
#3222=EDGE_CURVE('',#2652,#2650,#11,.T.);
#3223=EDGE_CURVE('',#2653,#2652,#2304,.T.);
#3224=EDGE_CURVE('',#2653,#2654,#1698,.T.);
#3225=EDGE_CURVE('',#2654,#2654,#2305,.T.);
#3226=EDGE_CURVE('',#2655,#2653,#2306,.T.);
#3227=EDGE_CURVE('',#2651,#2655,#12,.T.);
#3228=EDGE_CURVE('',#2655,#2652,#1699,.T.);
#3229=EDGE_CURVE('',#2656,#2656,#2307,.T.);
#3230=EDGE_CURVE('',#2656,#2657,#1700,.T.);
#3231=EDGE_CURVE('',#2657,#2657,#2308,.T.);
#3232=EDGE_CURVE('',#2658,#2659,#1701,.T.);
#3233=EDGE_CURVE('',#2660,#2658,#1702,.T.);
#3234=EDGE_CURVE('',#2661,#2660,#1703,.T.);
#3235=EDGE_CURVE('',#2659,#2661,#1704,.T.);
#3236=EDGE_CURVE('',#2662,#2658,#1705,.T.);
#3237=EDGE_CURVE('',#2663,#2662,#1706,.T.);
#3238=EDGE_CURVE('',#2660,#2663,#1707,.T.);
#3239=EDGE_CURVE('',#2664,#2662,#1708,.T.);
#3240=EDGE_CURVE('',#2665,#2664,#1709,.T.);
#3241=EDGE_CURVE('',#2663,#2665,#1710,.T.);
#3242=EDGE_CURVE('',#2666,#2665,#1711,.T.);
#3243=EDGE_CURVE('',#2667,#2666,#1712,.T.);
#3244=EDGE_CURVE('',#2668,#2667,#1713,.T.);
#3245=EDGE_CURVE('',#2669,#2668,#1714,.T.);
#3246=EDGE_CURVE('',#2661,#2669,#1715,.T.);
#3247=EDGE_CURVE('',#2670,#2664,#1716,.T.);
#3248=EDGE_CURVE('',#2666,#2670,#1717,.T.);
#3249=EDGE_CURVE('',#2669,#2671,#1718,.T.);
#3250=EDGE_CURVE('',#2659,#2671,#1719,.T.);
#3251=EDGE_CURVE('',#2667,#2672,#1720,.T.);
#3252=EDGE_CURVE('',#2673,#2672,#1721,.T.);
#3253=EDGE_CURVE('',#2668,#2673,#1722,.T.);
#3254=EDGE_CURVE('',#2671,#2673,#1723,.T.);
#3255=EDGE_CURVE('',#2672,#2670,#1724,.T.);
#3256=EDGE_CURVE('',#2674,#2675,#1725,.T.);
#3257=EDGE_CURVE('',#2674,#2676,#1726,.T.);
#3258=EDGE_CURVE('',#2676,#2677,#1727,.T.);
#3259=EDGE_CURVE('',#2675,#2677,#1728,.T.);
#3260=EDGE_CURVE('',#2678,#2674,#1729,.T.);
#3261=EDGE_CURVE('',#2678,#2679,#1730,.T.);
#3262=EDGE_CURVE('',#2679,#2676,#1731,.T.);
#3263=EDGE_CURVE('',#2680,#2678,#1732,.T.);
#3264=EDGE_CURVE('',#2680,#2681,#1733,.T.);
#3265=EDGE_CURVE('',#2681,#2679,#1734,.T.);
#3266=EDGE_CURVE('',#2682,#2680,#1735,.T.);
#3267=EDGE_CURVE('',#2682,#2683,#1736,.T.);
#3268=EDGE_CURVE('',#2683,#2681,#1737,.T.);
#3269=EDGE_CURVE('',#2684,#2682,#1738,.T.);
#3270=EDGE_CURVE('',#2684,#2685,#1739,.T.);
#3271=EDGE_CURVE('',#2685,#2683,#1740,.T.);
#3272=EDGE_CURVE('',#2675,#2684,#1741,.T.);
#3273=EDGE_CURVE('',#2677,#2685,#1742,.T.);
#3274=EDGE_CURVE('',#2686,#2686,#2309,.T.);
#3275=EDGE_CURVE('',#2687,#2687,#2310,.T.);
#3276=EDGE_CURVE('',#2687,#2686,#1743,.T.);
#3277=EDGE_CURVE('',#2688,#2688,#2311,.F.);
#3278=EDGE_CURVE('',#2688,#2687,#1744,.T.);
#3279=EDGE_CURVE('',#2689,#2689,#2312,.T.);
#3280=EDGE_CURVE('',#2689,#2688,#1745,.T.);
#3281=EDGE_CURVE('',#2690,#2691,#13,.T.);
#3282=EDGE_CURVE('',#2690,#2692,#1746,.T.);
#3283=EDGE_CURVE('',#2692,#2692,#14,.T.);
#3284=EDGE_CURVE('',#2693,#2690,#15,.T.);
#3285=EDGE_CURVE('',#2691,#2693,#16,.T.);
#3286=EDGE_CURVE('',#2694,#2694,#2313,.T.);
#3287=EDGE_CURVE('',#2695,#2695,#2314,.T.);
#3288=EDGE_CURVE('',#2695,#2694,#1747,.T.);
#3289=EDGE_CURVE('',#2696,#2696,#2315,.T.);
#3290=EDGE_CURVE('',#2696,#2695,#1748,.T.);
#3291=EDGE_CURVE('',#2697,#2697,#2316,.T.);
#3292=EDGE_CURVE('',#2698,#2698,#2317,.T.);
#3293=EDGE_CURVE('',#2698,#2691,#1749,.T.);
#3294=EDGE_CURVE('',#2693,#2697,#1750,.T.);
#3295=EDGE_CURVE('',#2699,#2699,#2318,.T.);
#3296=EDGE_CURVE('',#2699,#2698,#1751,.T.);
#3297=EDGE_CURVE('',#2700,#2700,#2319,.T.);
#3298=EDGE_CURVE('',#2700,#2701,#1752,.T.);
#3299=EDGE_CURVE('',#2701,#2701,#2320,.T.);
#3300=EDGE_CURVE('',#2702,#2702,#2321,.T.);
#3301=EDGE_CURVE('',#2702,#2703,#1753,.T.);
#3302=EDGE_CURVE('',#2703,#2703,#2322,.T.);
#3303=EDGE_CURVE('',#2704,#2704,#2323,.T.);
#3304=EDGE_CURVE('',#2704,#2704,#2324,.T.);
#3305=EDGE_CURVE('',#2705,#2706,#17,.T.);
#3306=EDGE_CURVE('',#2706,#2705,#18,.T.);
#3307=EDGE_CURVE('',#2707,#2708,#2325,.T.);
#3308=EDGE_CURVE('',#2707,#2708,#1754,.T.);
#3309=EDGE_CURVE('',#2708,#2709,#1755,.T.);
#3310=EDGE_CURVE('',#2710,#2709,#1756,.T.);
#3311=EDGE_CURVE('',#2707,#2710,#1757,.T.);
#3312=EDGE_CURVE('',#2711,#2710,#2326,.T.);
#3313=EDGE_CURVE('',#2711,#2706,#1758,.T.);
#3314=EDGE_CURVE('',#2709,#2711,#2327,.T.);
#3315=ORIENTED_EDGE('',*,*,#2712,.F.);
#3316=ORIENTED_EDGE('',*,*,#2713,.T.);
#3317=ORIENTED_EDGE('',*,*,#2714,.T.);
#3318=ORIENTED_EDGE('',*,*,#2713,.F.);
#3319=ORIENTED_EDGE('',*,*,#2714,.F.);
#3320=ORIENTED_EDGE('',*,*,#2715,.F.);
#3321=ORIENTED_EDGE('',*,*,#2716,.T.);
#3322=ORIENTED_EDGE('',*,*,#2717,.T.);
#3323=ORIENTED_EDGE('',*,*,#2716,.F.);
#3324=ORIENTED_EDGE('',*,*,#2717,.F.);
#3325=ORIENTED_EDGE('',*,*,#2718,.F.);
#3326=ORIENTED_EDGE('',*,*,#2719,.T.);
#3327=ORIENTED_EDGE('',*,*,#2720,.F.);
#3328=ORIENTED_EDGE('',*,*,#2721,.T.);
#3329=ORIENTED_EDGE('',*,*,#2722,.F.);
#3330=ORIENTED_EDGE('',*,*,#2723,.F.);
#3331=ORIENTED_EDGE('',*,*,#2721,.F.);
#3332=ORIENTED_EDGE('',*,*,#2724,.F.);
#3333=ORIENTED_EDGE('',*,*,#2719,.F.);
#3334=ORIENTED_EDGE('',*,*,#2725,.F.);
#3335=ORIENTED_EDGE('',*,*,#2726,.F.);
#3336=ORIENTED_EDGE('',*,*,#2727,.F.);
#3337=ORIENTED_EDGE('',*,*,#2728,.T.);
#3338=ORIENTED_EDGE('',*,*,#2729,.F.);
#3339=ORIENTED_EDGE('',*,*,#2730,.F.);
#3340=ORIENTED_EDGE('',*,*,#2731,.T.);
#3341=ORIENTED_EDGE('',*,*,#2732,.F.);
#3342=ORIENTED_EDGE('',*,*,#2733,.F.);
#3343=ORIENTED_EDGE('',*,*,#2728,.F.);
#3344=ORIENTED_EDGE('',*,*,#2734,.F.);
#3345=ORIENTED_EDGE('',*,*,#2735,.F.);
#3346=ORIENTED_EDGE('',*,*,#2736,.F.);
#3347=ORIENTED_EDGE('',*,*,#2737,.F.);
#3348=ORIENTED_EDGE('',*,*,#2738,.F.);
#3349=ORIENTED_EDGE('',*,*,#2731,.F.);
#3350=ORIENTED_EDGE('',*,*,#2739,.F.);
#3351=ORIENTED_EDGE('',*,*,#2736,.T.);
#3352=ORIENTED_EDGE('',*,*,#2725,.T.);
#3353=ORIENTED_EDGE('',*,*,#2740,.T.);
#3354=ORIENTED_EDGE('',*,*,#2718,.T.);
#3355=ORIENTED_EDGE('',*,*,#2741,.T.);
#3356=ORIENTED_EDGE('',*,*,#2726,.T.);
#3357=ORIENTED_EDGE('',*,*,#2740,.F.);
#3358=ORIENTED_EDGE('',*,*,#2723,.T.);
#3359=ORIENTED_EDGE('',*,*,#2739,.T.);
#3360=ORIENTED_EDGE('',*,*,#2735,.T.);
#3361=ORIENTED_EDGE('',*,*,#2742,.T.);
#3362=ORIENTED_EDGE('',*,*,#2743,.F.);
#3363=ORIENTED_EDGE('',*,*,#2742,.F.);
#3364=ORIENTED_EDGE('',*,*,#2727,.T.);
#3365=ORIENTED_EDGE('',*,*,#2722,.T.);
#3366=ORIENTED_EDGE('',*,*,#2720,.T.);
#3367=ORIENTED_EDGE('',*,*,#2741,.F.);
#3368=ORIENTED_EDGE('',*,*,#2734,.T.);
#3369=ORIENTED_EDGE('',*,*,#2737,.T.);
#3370=ORIENTED_EDGE('',*,*,#2744,.F.);
#3371=ORIENTED_EDGE('',*,*,#2732,.T.);
#3372=ORIENTED_EDGE('',*,*,#2738,.T.);
#3373=ORIENTED_EDGE('',*,*,#2730,.T.);
#3374=ORIENTED_EDGE('',*,*,#2745,.F.);
#3375=ORIENTED_EDGE('',*,*,#2746,.T.);
#3376=ORIENTED_EDGE('',*,*,#2747,.F.);
#3377=ORIENTED_EDGE('',*,*,#2746,.F.);
#3378=ORIENTED_EDGE('',*,*,#2748,.F.);
#3379=ORIENTED_EDGE('',*,*,#2724,.T.);
#3380=ORIENTED_EDGE('',*,*,#2744,.T.);
#3381=ORIENTED_EDGE('',*,*,#2749,.F.);
#3382=ORIENTED_EDGE('',*,*,#2750,.T.);
#3383=ORIENTED_EDGE('',*,*,#2751,.F.);
#3384=ORIENTED_EDGE('',*,*,#2750,.F.);
#3385=ORIENTED_EDGE('',*,*,#2749,.T.);
#3386=ORIENTED_EDGE('',*,*,#2743,.T.);
#3387=ORIENTED_EDGE('',*,*,#2752,.F.);
#3388=ORIENTED_EDGE('',*,*,#2753,.T.);
#3389=ORIENTED_EDGE('',*,*,#2754,.F.);
#3390=ORIENTED_EDGE('',*,*,#2753,.F.);
#3391=ORIENTED_EDGE('',*,*,#2755,.F.);
#3392=ORIENTED_EDGE('',*,*,#2756,.T.);
#3393=ORIENTED_EDGE('',*,*,#2757,.F.);
#3394=ORIENTED_EDGE('',*,*,#2756,.F.);
#3395=ORIENTED_EDGE('',*,*,#2758,.F.);
#3396=ORIENTED_EDGE('',*,*,#2759,.T.);
#3397=ORIENTED_EDGE('',*,*,#2760,.F.);
#3398=ORIENTED_EDGE('',*,*,#2759,.F.);
#3399=ORIENTED_EDGE('',*,*,#2761,.F.);
#3400=ORIENTED_EDGE('',*,*,#2762,.T.);
#3401=ORIENTED_EDGE('',*,*,#2763,.F.);
#3402=ORIENTED_EDGE('',*,*,#2762,.F.);
#3403=ORIENTED_EDGE('',*,*,#2764,.F.);
#3404=ORIENTED_EDGE('',*,*,#2765,.T.);
#3405=ORIENTED_EDGE('',*,*,#2766,.F.);
#3406=ORIENTED_EDGE('',*,*,#2765,.F.);
#3407=ORIENTED_EDGE('',*,*,#2729,.T.);
#3408=ORIENTED_EDGE('',*,*,#2733,.T.);
#3409=ORIENTED_EDGE('',*,*,#2748,.T.);
#3410=ORIENTED_EDGE('',*,*,#2745,.T.);
#3411=ORIENTED_EDGE('',*,*,#2766,.T.);
#3412=ORIENTED_EDGE('',*,*,#2767,.T.);
#3413=ORIENTED_EDGE('',*,*,#2768,.T.);
#3414=ORIENTED_EDGE('',*,*,#2769,.F.);
#3415=ORIENTED_EDGE('',*,*,#2770,.F.);
#3416=ORIENTED_EDGE('',*,*,#2747,.T.);
#3417=ORIENTED_EDGE('',*,*,#2763,.T.);
#3418=ORIENTED_EDGE('',*,*,#2760,.T.);
#3419=ORIENTED_EDGE('',*,*,#2757,.T.);
#3420=ORIENTED_EDGE('',*,*,#2754,.T.);
#3421=ORIENTED_EDGE('',*,*,#2771,.T.);
#3422=ORIENTED_EDGE('',*,*,#2770,.T.);
#3423=ORIENTED_EDGE('',*,*,#2772,.F.);
#3424=ORIENTED_EDGE('',*,*,#2773,.F.);
#3425=ORIENTED_EDGE('',*,*,#2774,.T.);
#3426=ORIENTED_EDGE('',*,*,#2773,.T.);
#3427=ORIENTED_EDGE('',*,*,#2775,.F.);
#3428=ORIENTED_EDGE('',*,*,#2776,.F.);
#3429=ORIENTED_EDGE('',*,*,#2764,.T.);
#3430=ORIENTED_EDGE('',*,*,#2761,.T.);
#3431=ORIENTED_EDGE('',*,*,#2758,.T.);
#3432=ORIENTED_EDGE('',*,*,#2755,.T.);
#3433=ORIENTED_EDGE('',*,*,#2752,.T.);
#3434=ORIENTED_EDGE('',*,*,#2777,.T.);
#3435=ORIENTED_EDGE('',*,*,#2776,.T.);
#3436=ORIENTED_EDGE('',*,*,#2778,.F.);
#3437=ORIENTED_EDGE('',*,*,#2768,.F.);
#3438=ORIENTED_EDGE('',*,*,#2778,.T.);
#3439=ORIENTED_EDGE('',*,*,#2775,.T.);
#3440=ORIENTED_EDGE('',*,*,#2772,.T.);
#3441=ORIENTED_EDGE('',*,*,#2769,.T.);
#3442=ORIENTED_EDGE('',*,*,#2751,.T.);
#3443=ORIENTED_EDGE('',*,*,#2777,.F.);
#3444=ORIENTED_EDGE('',*,*,#2767,.F.);
#3445=ORIENTED_EDGE('',*,*,#2771,.F.);
#3446=ORIENTED_EDGE('',*,*,#2774,.F.);
#3447=ORIENTED_EDGE('',*,*,#2712,.T.);
#3448=ORIENTED_EDGE('',*,*,#2715,.T.);
#3449=ORIENTED_EDGE('',*,*,#2779,.F.);
#3450=ORIENTED_EDGE('',*,*,#2780,.T.);
#3451=ORIENTED_EDGE('',*,*,#2781,.F.);
#3452=ORIENTED_EDGE('',*,*,#2780,.F.);
#3453=ORIENTED_EDGE('',*,*,#2779,.T.);
#3454=ORIENTED_EDGE('',*,*,#2782,.F.);
#3455=ORIENTED_EDGE('',*,*,#2783,.F.);
#3456=ORIENTED_EDGE('',*,*,#2784,.F.);
#3457=ORIENTED_EDGE('',*,*,#2785,.F.);
#3458=ORIENTED_EDGE('',*,*,#2783,.T.);
#3459=ORIENTED_EDGE('',*,*,#2786,.F.);
#3460=ORIENTED_EDGE('',*,*,#2787,.T.);
#3461=ORIENTED_EDGE('',*,*,#2784,.T.);
#3462=ORIENTED_EDGE('',*,*,#2786,.T.);
#3463=ORIENTED_EDGE('',*,*,#2782,.T.);
#3464=ORIENTED_EDGE('',*,*,#2788,.F.);
#3465=ORIENTED_EDGE('',*,*,#2789,.F.);
#3466=ORIENTED_EDGE('',*,*,#2790,.T.);
#3467=ORIENTED_EDGE('',*,*,#2791,.T.);
#3468=ORIENTED_EDGE('',*,*,#2790,.F.);
#3469=ORIENTED_EDGE('',*,*,#2791,.F.);
#3470=ORIENTED_EDGE('',*,*,#2792,.F.);
#3471=ORIENTED_EDGE('',*,*,#2789,.T.);
#3472=ORIENTED_EDGE('',*,*,#2793,.F.);
#3473=ORIENTED_EDGE('',*,*,#2787,.F.);
#3474=ORIENTED_EDGE('',*,*,#2794,.T.);
#3475=ORIENTED_EDGE('',*,*,#2793,.T.);
#3476=ORIENTED_EDGE('',*,*,#2794,.F.);
#3477=ORIENTED_EDGE('',*,*,#2792,.T.);
#3478=ORIENTED_EDGE('',*,*,#2795,.T.);
#3479=ORIENTED_EDGE('',*,*,#2796,.F.);
#3480=ORIENTED_EDGE('',*,*,#2795,.F.);
#3481=ORIENTED_EDGE('',*,*,#2785,.T.);
#3482=ORIENTED_EDGE('',*,*,#2788,.T.);
#3483=ORIENTED_EDGE('',*,*,#2797,.F.);
#3484=ORIENTED_EDGE('',*,*,#2798,.T.);
#3485=ORIENTED_EDGE('',*,*,#2799,.T.);
#3486=ORIENTED_EDGE('',*,*,#2800,.T.);
#3487=ORIENTED_EDGE('',*,*,#2801,.F.);
#3488=ORIENTED_EDGE('',*,*,#2802,.F.);
#3489=ORIENTED_EDGE('',*,*,#2803,.F.);
#3490=ORIENTED_EDGE('',*,*,#2804,.T.);
#3491=ORIENTED_EDGE('',*,*,#2805,.T.);
#3492=ORIENTED_EDGE('',*,*,#2806,.F.);
#3493=ORIENTED_EDGE('',*,*,#2807,.F.);
#3494=ORIENTED_EDGE('',*,*,#2801,.T.);
#3495=ORIENTED_EDGE('',*,*,#2808,.F.);
#3496=ORIENTED_EDGE('',*,*,#2809,.T.);
#3497=ORIENTED_EDGE('',*,*,#2807,.T.);
#3498=ORIENTED_EDGE('',*,*,#2810,.F.);
#3499=ORIENTED_EDGE('',*,*,#2811,.F.);
#3500=ORIENTED_EDGE('',*,*,#2781,.T.);
#3501=ORIENTED_EDGE('',*,*,#2802,.T.);
#3502=ORIENTED_EDGE('',*,*,#2811,.T.);
#3503=ORIENTED_EDGE('',*,*,#2812,.F.);
#3504=ORIENTED_EDGE('',*,*,#2813,.F.);
#3505=ORIENTED_EDGE('',*,*,#2814,.T.);
#3506=ORIENTED_EDGE('',*,*,#2815,.F.);
#3507=ORIENTED_EDGE('',*,*,#2803,.T.);
#3508=ORIENTED_EDGE('',*,*,#2813,.T.);
#3509=ORIENTED_EDGE('',*,*,#2816,.F.);
#3510=ORIENTED_EDGE('',*,*,#2805,.F.);
#3511=ORIENTED_EDGE('',*,*,#2816,.T.);
#3512=ORIENTED_EDGE('',*,*,#2812,.T.);
#3513=ORIENTED_EDGE('',*,*,#2810,.T.);
#3514=ORIENTED_EDGE('',*,*,#2806,.T.);
#3515=ORIENTED_EDGE('',*,*,#2796,.T.);
#3516=ORIENTED_EDGE('',*,*,#2817,.T.);
#3517=ORIENTED_EDGE('',*,*,#2814,.F.);
#3518=ORIENTED_EDGE('',*,*,#2804,.F.);
#3519=ORIENTED_EDGE('',*,*,#2809,.F.);
#3520=ORIENTED_EDGE('',*,*,#2818,.T.);
#3521=ORIENTED_EDGE('',*,*,#2819,.T.);
#3522=ORIENTED_EDGE('',*,*,#2808,.T.);
#3523=ORIENTED_EDGE('',*,*,#2820,.T.);
#3524=ORIENTED_EDGE('',*,*,#2821,.T.);
#3525=ORIENTED_EDGE('',*,*,#2822,.F.);
#3526=ORIENTED_EDGE('',*,*,#2823,.F.);
#3527=ORIENTED_EDGE('',*,*,#2824,.F.);
#3528=ORIENTED_EDGE('',*,*,#2825,.F.);
#3529=ORIENTED_EDGE('',*,*,#2826,.F.);
#3530=ORIENTED_EDGE('',*,*,#2827,.F.);
#3531=ORIENTED_EDGE('',*,*,#2828,.T.);
#3532=ORIENTED_EDGE('',*,*,#2823,.T.);
#3533=ORIENTED_EDGE('',*,*,#2829,.T.);
#3534=ORIENTED_EDGE('',*,*,#2799,.F.);
#3535=ORIENTED_EDGE('',*,*,#2830,.F.);
#3536=ORIENTED_EDGE('',*,*,#2824,.T.);
#3537=ORIENTED_EDGE('',*,*,#2830,.T.);
#3538=ORIENTED_EDGE('',*,*,#2798,.F.);
#3539=ORIENTED_EDGE('',*,*,#2831,.F.);
#3540=ORIENTED_EDGE('',*,*,#2832,.F.);
#3541=ORIENTED_EDGE('',*,*,#2825,.T.);
#3542=ORIENTED_EDGE('',*,*,#2832,.T.);
#3543=ORIENTED_EDGE('',*,*,#2833,.F.);
#3544=ORIENTED_EDGE('',*,*,#2817,.F.);
#3545=ORIENTED_EDGE('',*,*,#2834,.F.);
#3546=ORIENTED_EDGE('',*,*,#2826,.T.);
#3547=ORIENTED_EDGE('',*,*,#2834,.T.);
#3548=ORIENTED_EDGE('',*,*,#2819,.F.);
#3549=ORIENTED_EDGE('',*,*,#2835,.F.);
#3550=ORIENTED_EDGE('',*,*,#2827,.T.);
#3551=ORIENTED_EDGE('',*,*,#2835,.T.);
#3552=ORIENTED_EDGE('',*,*,#2818,.F.);
#3553=ORIENTED_EDGE('',*,*,#2821,.F.);
#3554=ORIENTED_EDGE('',*,*,#2836,.F.);
#3555=ORIENTED_EDGE('',*,*,#2822,.T.);
#3556=ORIENTED_EDGE('',*,*,#2836,.T.);
#3557=ORIENTED_EDGE('',*,*,#2820,.F.);
#3558=ORIENTED_EDGE('',*,*,#2800,.F.);
#3559=ORIENTED_EDGE('',*,*,#2829,.F.);
#3560=ORIENTED_EDGE('',*,*,#2815,.T.);
#3561=ORIENTED_EDGE('',*,*,#2833,.T.);
#3562=ORIENTED_EDGE('',*,*,#2831,.T.);
#3563=ORIENTED_EDGE('',*,*,#2797,.T.);
#3564=ORIENTED_EDGE('',*,*,#2837,.T.);
#3565=ORIENTED_EDGE('',*,*,#2838,.T.);
#3566=ORIENTED_EDGE('',*,*,#2837,.F.);
#3567=ORIENTED_EDGE('',*,*,#2828,.F.);
#3568=ORIENTED_EDGE('',*,*,#2839,.T.);
#3569=ORIENTED_EDGE('',*,*,#2840,.T.);
#3570=ORIENTED_EDGE('',*,*,#2839,.F.);
#3571=ORIENTED_EDGE('',*,*,#2840,.F.);
#3572=ORIENTED_EDGE('',*,*,#2838,.F.);
#3573=ORIENTED_EDGE('',*,*,#2841,.F.);
#3574=ORIENTED_EDGE('',*,*,#2842,.T.);
#3575=ORIENTED_EDGE('',*,*,#2842,.F.);
#3576=ORIENTED_EDGE('',*,*,#2843,.F.);
#3577=ORIENTED_EDGE('',*,*,#2844,.T.);
#3578=ORIENTED_EDGE('',*,*,#2841,.T.);
#3579=ORIENTED_EDGE('',*,*,#2844,.F.);
#3580=ORIENTED_EDGE('',*,*,#2845,.F.);
#3581=ORIENTED_EDGE('',*,*,#2846,.T.);
#3582=ORIENTED_EDGE('',*,*,#2843,.T.);
#3583=ORIENTED_EDGE('',*,*,#2846,.F.);
#3584=ORIENTED_EDGE('',*,*,#2847,.F.);
#3585=ORIENTED_EDGE('',*,*,#2845,.T.);
#3586=ORIENTED_EDGE('',*,*,#2848,.F.);
#3587=ORIENTED_EDGE('',*,*,#2849,.T.);
#3588=ORIENTED_EDGE('',*,*,#2847,.T.);
#3589=ORIENTED_EDGE('',*,*,#2849,.F.);
#3590=ORIENTED_EDGE('',*,*,#2848,.T.);
#3591=ORIENTED_EDGE('',*,*,#2850,.F.);
#3592=ORIENTED_EDGE('',*,*,#2851,.T.);
#3593=ORIENTED_EDGE('',*,*,#2852,.T.);
#3594=ORIENTED_EDGE('',*,*,#2851,.F.);
#3595=ORIENTED_EDGE('',*,*,#2852,.F.);
#3596=ORIENTED_EDGE('',*,*,#2853,.F.);
#3597=ORIENTED_EDGE('',*,*,#2854,.T.);
#3598=ORIENTED_EDGE('',*,*,#2855,.T.);
#3599=ORIENTED_EDGE('',*,*,#2854,.F.);
#3600=ORIENTED_EDGE('',*,*,#2855,.F.);
#3601=ORIENTED_EDGE('',*,*,#2856,.F.);
#3602=ORIENTED_EDGE('',*,*,#2857,.F.);
#3603=ORIENTED_EDGE('',*,*,#2858,.F.);
#3604=ORIENTED_EDGE('',*,*,#2859,.F.);
#3605=ORIENTED_EDGE('',*,*,#2860,.F.);
#3606=ORIENTED_EDGE('',*,*,#2861,.F.);
#3607=ORIENTED_EDGE('',*,*,#2862,.F.);
#3608=ORIENTED_EDGE('',*,*,#2863,.F.);
#3609=ORIENTED_EDGE('',*,*,#2864,.F.);
#3610=ORIENTED_EDGE('',*,*,#2865,.F.);
#3611=ORIENTED_EDGE('',*,*,#2866,.T.);
#3612=ORIENTED_EDGE('',*,*,#2867,.F.);
#3613=ORIENTED_EDGE('',*,*,#2868,.F.);
#3614=ORIENTED_EDGE('',*,*,#2869,.F.);
#3615=ORIENTED_EDGE('',*,*,#2857,.T.);
#3616=ORIENTED_EDGE('',*,*,#2870,.F.);
#3617=ORIENTED_EDGE('',*,*,#2871,.F.);
#3618=ORIENTED_EDGE('',*,*,#2866,.F.);
#3619=ORIENTED_EDGE('',*,*,#2872,.F.);
#3620=ORIENTED_EDGE('',*,*,#2873,.F.);
#3621=ORIENTED_EDGE('',*,*,#2859,.T.);
#3622=ORIENTED_EDGE('',*,*,#2874,.F.);
#3623=ORIENTED_EDGE('',*,*,#2875,.F.);
#3624=ORIENTED_EDGE('',*,*,#2876,.F.);
#3625=ORIENTED_EDGE('',*,*,#2861,.T.);
#3626=ORIENTED_EDGE('',*,*,#2877,.F.);
#3627=ORIENTED_EDGE('',*,*,#2863,.T.);
#3628=ORIENTED_EDGE('',*,*,#2856,.T.);
#3629=ORIENTED_EDGE('',*,*,#2878,.T.);
#3630=ORIENTED_EDGE('',*,*,#2869,.T.);
#3631=ORIENTED_EDGE('',*,*,#2879,.T.);
#3632=ORIENTED_EDGE('',*,*,#2870,.T.);
#3633=ORIENTED_EDGE('',*,*,#2880,.T.);
#3634=ORIENTED_EDGE('',*,*,#2874,.T.);
#3635=ORIENTED_EDGE('',*,*,#2879,.F.);
#3636=ORIENTED_EDGE('',*,*,#2868,.T.);
#3637=ORIENTED_EDGE('',*,*,#2871,.T.);
#3638=ORIENTED_EDGE('',*,*,#2880,.F.);
#3639=ORIENTED_EDGE('',*,*,#2876,.T.);
#3640=ORIENTED_EDGE('',*,*,#2860,.T.);
#3641=ORIENTED_EDGE('',*,*,#2878,.F.);
#3642=ORIENTED_EDGE('',*,*,#2858,.T.);
#3643=ORIENTED_EDGE('',*,*,#2873,.T.);
#3644=ORIENTED_EDGE('',*,*,#2867,.T.);
#3645=ORIENTED_EDGE('',*,*,#2881,.T.);
#3646=ORIENTED_EDGE('',*,*,#2882,.F.);
#3647=ORIENTED_EDGE('',*,*,#2881,.F.);
#3648=ORIENTED_EDGE('',*,*,#2875,.T.);
#3649=ORIENTED_EDGE('',*,*,#2872,.T.);
#3650=ORIENTED_EDGE('',*,*,#2865,.T.);
#3651=ORIENTED_EDGE('',*,*,#2883,.F.);
#3652=ORIENTED_EDGE('',*,*,#2884,.F.);
#3653=ORIENTED_EDGE('',*,*,#2885,.F.);
#3654=ORIENTED_EDGE('',*,*,#2886,.T.);
#3655=ORIENTED_EDGE('',*,*,#2887,.F.);
#3656=ORIENTED_EDGE('',*,*,#2886,.F.);
#3657=ORIENTED_EDGE('',*,*,#2885,.T.);
#3658=ORIENTED_EDGE('',*,*,#2882,.T.);
#3659=ORIENTED_EDGE('',*,*,#2888,.F.);
#3660=ORIENTED_EDGE('',*,*,#2889,.T.);
#3661=ORIENTED_EDGE('',*,*,#2890,.F.);
#3662=ORIENTED_EDGE('',*,*,#2889,.F.);
#3663=ORIENTED_EDGE('',*,*,#2891,.F.);
#3664=ORIENTED_EDGE('',*,*,#2892,.T.);
#3665=ORIENTED_EDGE('',*,*,#2893,.F.);
#3666=ORIENTED_EDGE('',*,*,#2892,.F.);
#3667=ORIENTED_EDGE('',*,*,#2894,.F.);
#3668=ORIENTED_EDGE('',*,*,#2895,.T.);
#3669=ORIENTED_EDGE('',*,*,#2896,.F.);
#3670=ORIENTED_EDGE('',*,*,#2895,.F.);
#3671=ORIENTED_EDGE('',*,*,#2897,.F.);
#3672=ORIENTED_EDGE('',*,*,#2898,.T.);
#3673=ORIENTED_EDGE('',*,*,#2899,.F.);
#3674=ORIENTED_EDGE('',*,*,#2898,.F.);
#3675=ORIENTED_EDGE('',*,*,#2900,.F.);
#3676=ORIENTED_EDGE('',*,*,#2901,.T.);
#3677=ORIENTED_EDGE('',*,*,#2883,.T.);
#3678=ORIENTED_EDGE('',*,*,#2864,.T.);
#3679=ORIENTED_EDGE('',*,*,#2877,.T.);
#3680=ORIENTED_EDGE('',*,*,#2862,.T.);
#3681=ORIENTED_EDGE('',*,*,#2884,.T.);
#3682=ORIENTED_EDGE('',*,*,#2901,.F.);
#3683=ORIENTED_EDGE('',*,*,#2902,.T.);
#3684=ORIENTED_EDGE('',*,*,#2903,.T.);
#3685=ORIENTED_EDGE('',*,*,#2904,.F.);
#3686=ORIENTED_EDGE('',*,*,#2905,.F.);
#3687=ORIENTED_EDGE('',*,*,#2890,.T.);
#3688=ORIENTED_EDGE('',*,*,#2893,.T.);
#3689=ORIENTED_EDGE('',*,*,#2896,.T.);
#3690=ORIENTED_EDGE('',*,*,#2899,.T.);
#3691=ORIENTED_EDGE('',*,*,#2906,.T.);
#3692=ORIENTED_EDGE('',*,*,#2905,.T.);
#3693=ORIENTED_EDGE('',*,*,#2907,.F.);
#3694=ORIENTED_EDGE('',*,*,#2908,.F.);
#3695=ORIENTED_EDGE('',*,*,#2909,.T.);
#3696=ORIENTED_EDGE('',*,*,#2908,.T.);
#3697=ORIENTED_EDGE('',*,*,#2910,.F.);
#3698=ORIENTED_EDGE('',*,*,#2911,.F.);
#3699=ORIENTED_EDGE('',*,*,#2900,.T.);
#3700=ORIENTED_EDGE('',*,*,#2897,.T.);
#3701=ORIENTED_EDGE('',*,*,#2894,.T.);
#3702=ORIENTED_EDGE('',*,*,#2891,.T.);
#3703=ORIENTED_EDGE('',*,*,#2888,.T.);
#3704=ORIENTED_EDGE('',*,*,#2912,.T.);
#3705=ORIENTED_EDGE('',*,*,#2911,.T.);
#3706=ORIENTED_EDGE('',*,*,#2913,.F.);
#3707=ORIENTED_EDGE('',*,*,#2903,.F.);
#3708=ORIENTED_EDGE('',*,*,#2913,.T.);
#3709=ORIENTED_EDGE('',*,*,#2910,.T.);
#3710=ORIENTED_EDGE('',*,*,#2907,.T.);
#3711=ORIENTED_EDGE('',*,*,#2904,.T.);
#3712=ORIENTED_EDGE('',*,*,#2887,.T.);
#3713=ORIENTED_EDGE('',*,*,#2912,.F.);
#3714=ORIENTED_EDGE('',*,*,#2902,.F.);
#3715=ORIENTED_EDGE('',*,*,#2906,.F.);
#3716=ORIENTED_EDGE('',*,*,#2909,.F.);
#3717=ORIENTED_EDGE('',*,*,#2850,.T.);
#3718=ORIENTED_EDGE('',*,*,#2853,.T.);
#3719=ORIENTED_EDGE('',*,*,#2914,.F.);
#3720=ORIENTED_EDGE('',*,*,#2915,.T.);
#3721=ORIENTED_EDGE('',*,*,#2916,.F.);
#3722=ORIENTED_EDGE('',*,*,#2915,.F.);
#3723=ORIENTED_EDGE('',*,*,#2914,.T.);
#3724=ORIENTED_EDGE('',*,*,#2917,.F.);
#3725=ORIENTED_EDGE('',*,*,#2918,.F.);
#3726=ORIENTED_EDGE('',*,*,#2919,.F.);
#3727=ORIENTED_EDGE('',*,*,#2920,.F.);
#3728=ORIENTED_EDGE('',*,*,#2918,.T.);
#3729=ORIENTED_EDGE('',*,*,#2921,.F.);
#3730=ORIENTED_EDGE('',*,*,#2922,.T.);
#3731=ORIENTED_EDGE('',*,*,#2919,.T.);
#3732=ORIENTED_EDGE('',*,*,#2921,.T.);
#3733=ORIENTED_EDGE('',*,*,#2917,.T.);
#3734=ORIENTED_EDGE('',*,*,#2923,.F.);
#3735=ORIENTED_EDGE('',*,*,#2924,.F.);
#3736=ORIENTED_EDGE('',*,*,#2925,.T.);
#3737=ORIENTED_EDGE('',*,*,#2926,.T.);
#3738=ORIENTED_EDGE('',*,*,#2925,.F.);
#3739=ORIENTED_EDGE('',*,*,#2926,.F.);
#3740=ORIENTED_EDGE('',*,*,#2927,.F.);
#3741=ORIENTED_EDGE('',*,*,#2924,.T.);
#3742=ORIENTED_EDGE('',*,*,#2928,.F.);
#3743=ORIENTED_EDGE('',*,*,#2922,.F.);
#3744=ORIENTED_EDGE('',*,*,#2929,.T.);
#3745=ORIENTED_EDGE('',*,*,#2928,.T.);
#3746=ORIENTED_EDGE('',*,*,#2929,.F.);
#3747=ORIENTED_EDGE('',*,*,#2927,.T.);
#3748=ORIENTED_EDGE('',*,*,#2930,.T.);
#3749=ORIENTED_EDGE('',*,*,#2931,.F.);
#3750=ORIENTED_EDGE('',*,*,#2930,.F.);
#3751=ORIENTED_EDGE('',*,*,#2920,.T.);
#3752=ORIENTED_EDGE('',*,*,#2923,.T.);
#3753=ORIENTED_EDGE('',*,*,#2932,.F.);
#3754=ORIENTED_EDGE('',*,*,#2933,.T.);
#3755=ORIENTED_EDGE('',*,*,#2934,.T.);
#3756=ORIENTED_EDGE('',*,*,#2935,.T.);
#3757=ORIENTED_EDGE('',*,*,#2936,.F.);
#3758=ORIENTED_EDGE('',*,*,#2937,.F.);
#3759=ORIENTED_EDGE('',*,*,#2938,.F.);
#3760=ORIENTED_EDGE('',*,*,#2939,.T.);
#3761=ORIENTED_EDGE('',*,*,#2940,.T.);
#3762=ORIENTED_EDGE('',*,*,#2941,.F.);
#3763=ORIENTED_EDGE('',*,*,#2942,.F.);
#3764=ORIENTED_EDGE('',*,*,#2936,.T.);
#3765=ORIENTED_EDGE('',*,*,#2943,.F.);
#3766=ORIENTED_EDGE('',*,*,#2944,.T.);
#3767=ORIENTED_EDGE('',*,*,#2942,.T.);
#3768=ORIENTED_EDGE('',*,*,#2945,.F.);
#3769=ORIENTED_EDGE('',*,*,#2946,.F.);
#3770=ORIENTED_EDGE('',*,*,#2916,.T.);
#3771=ORIENTED_EDGE('',*,*,#2937,.T.);
#3772=ORIENTED_EDGE('',*,*,#2946,.T.);
#3773=ORIENTED_EDGE('',*,*,#2947,.F.);
#3774=ORIENTED_EDGE('',*,*,#2948,.F.);
#3775=ORIENTED_EDGE('',*,*,#2949,.T.);
#3776=ORIENTED_EDGE('',*,*,#2950,.F.);
#3777=ORIENTED_EDGE('',*,*,#2938,.T.);
#3778=ORIENTED_EDGE('',*,*,#2948,.T.);
#3779=ORIENTED_EDGE('',*,*,#2951,.F.);
#3780=ORIENTED_EDGE('',*,*,#2940,.F.);
#3781=ORIENTED_EDGE('',*,*,#2951,.T.);
#3782=ORIENTED_EDGE('',*,*,#2947,.T.);
#3783=ORIENTED_EDGE('',*,*,#2945,.T.);
#3784=ORIENTED_EDGE('',*,*,#2941,.T.);
#3785=ORIENTED_EDGE('',*,*,#2931,.T.);
#3786=ORIENTED_EDGE('',*,*,#2952,.T.);
#3787=ORIENTED_EDGE('',*,*,#2949,.F.);
#3788=ORIENTED_EDGE('',*,*,#2939,.F.);
#3789=ORIENTED_EDGE('',*,*,#2944,.F.);
#3790=ORIENTED_EDGE('',*,*,#2953,.T.);
#3791=ORIENTED_EDGE('',*,*,#2954,.T.);
#3792=ORIENTED_EDGE('',*,*,#2943,.T.);
#3793=ORIENTED_EDGE('',*,*,#2955,.T.);
#3794=ORIENTED_EDGE('',*,*,#2956,.T.);
#3795=ORIENTED_EDGE('',*,*,#2957,.F.);
#3796=ORIENTED_EDGE('',*,*,#2958,.F.);
#3797=ORIENTED_EDGE('',*,*,#2959,.F.);
#3798=ORIENTED_EDGE('',*,*,#2960,.F.);
#3799=ORIENTED_EDGE('',*,*,#2961,.F.);
#3800=ORIENTED_EDGE('',*,*,#2962,.F.);
#3801=ORIENTED_EDGE('',*,*,#2963,.T.);
#3802=ORIENTED_EDGE('',*,*,#2958,.T.);
#3803=ORIENTED_EDGE('',*,*,#2964,.T.);
#3804=ORIENTED_EDGE('',*,*,#2934,.F.);
#3805=ORIENTED_EDGE('',*,*,#2965,.F.);
#3806=ORIENTED_EDGE('',*,*,#2959,.T.);
#3807=ORIENTED_EDGE('',*,*,#2965,.T.);
#3808=ORIENTED_EDGE('',*,*,#2933,.F.);
#3809=ORIENTED_EDGE('',*,*,#2966,.F.);
#3810=ORIENTED_EDGE('',*,*,#2967,.F.);
#3811=ORIENTED_EDGE('',*,*,#2960,.T.);
#3812=ORIENTED_EDGE('',*,*,#2967,.T.);
#3813=ORIENTED_EDGE('',*,*,#2968,.F.);
#3814=ORIENTED_EDGE('',*,*,#2952,.F.);
#3815=ORIENTED_EDGE('',*,*,#2969,.F.);
#3816=ORIENTED_EDGE('',*,*,#2961,.T.);
#3817=ORIENTED_EDGE('',*,*,#2969,.T.);
#3818=ORIENTED_EDGE('',*,*,#2954,.F.);
#3819=ORIENTED_EDGE('',*,*,#2970,.F.);
#3820=ORIENTED_EDGE('',*,*,#2962,.T.);
#3821=ORIENTED_EDGE('',*,*,#2970,.T.);
#3822=ORIENTED_EDGE('',*,*,#2953,.F.);
#3823=ORIENTED_EDGE('',*,*,#2956,.F.);
#3824=ORIENTED_EDGE('',*,*,#2971,.F.);
#3825=ORIENTED_EDGE('',*,*,#2957,.T.);
#3826=ORIENTED_EDGE('',*,*,#2971,.T.);
#3827=ORIENTED_EDGE('',*,*,#2955,.F.);
#3828=ORIENTED_EDGE('',*,*,#2935,.F.);
#3829=ORIENTED_EDGE('',*,*,#2964,.F.);
#3830=ORIENTED_EDGE('',*,*,#2950,.T.);
#3831=ORIENTED_EDGE('',*,*,#2968,.T.);
#3832=ORIENTED_EDGE('',*,*,#2966,.T.);
#3833=ORIENTED_EDGE('',*,*,#2932,.T.);
#3834=ORIENTED_EDGE('',*,*,#2972,.T.);
#3835=ORIENTED_EDGE('',*,*,#2973,.T.);
#3836=ORIENTED_EDGE('',*,*,#2972,.F.);
#3837=ORIENTED_EDGE('',*,*,#2963,.F.);
#3838=ORIENTED_EDGE('',*,*,#2974,.T.);
#3839=ORIENTED_EDGE('',*,*,#2975,.T.);
#3840=ORIENTED_EDGE('',*,*,#2974,.F.);
#3841=ORIENTED_EDGE('',*,*,#2975,.F.);
#3842=ORIENTED_EDGE('',*,*,#2973,.F.);
#3843=ORIENTED_EDGE('',*,*,#2976,.F.);
#3844=ORIENTED_EDGE('',*,*,#2977,.T.);
#3845=ORIENTED_EDGE('',*,*,#2977,.F.);
#3846=ORIENTED_EDGE('',*,*,#2978,.F.);
#3847=ORIENTED_EDGE('',*,*,#2979,.T.);
#3848=ORIENTED_EDGE('',*,*,#2976,.T.);
#3849=ORIENTED_EDGE('',*,*,#2979,.F.);
#3850=ORIENTED_EDGE('',*,*,#2980,.F.);
#3851=ORIENTED_EDGE('',*,*,#2981,.T.);
#3852=ORIENTED_EDGE('',*,*,#2978,.T.);
#3853=ORIENTED_EDGE('',*,*,#2981,.F.);
#3854=ORIENTED_EDGE('',*,*,#2982,.F.);
#3855=ORIENTED_EDGE('',*,*,#2980,.T.);
#3856=ORIENTED_EDGE('',*,*,#2983,.F.);
#3857=ORIENTED_EDGE('',*,*,#2984,.T.);
#3858=ORIENTED_EDGE('',*,*,#2982,.T.);
#3859=ORIENTED_EDGE('',*,*,#2984,.F.);
#3860=ORIENTED_EDGE('',*,*,#2983,.T.);
#3861=ORIENTED_EDGE('',*,*,#2985,.F.);
#3862=ORIENTED_EDGE('',*,*,#2986,.T.);
#3863=ORIENTED_EDGE('',*,*,#2987,.T.);
#3864=ORIENTED_EDGE('',*,*,#2986,.F.);
#3865=ORIENTED_EDGE('',*,*,#2988,.F.);
#3866=ORIENTED_EDGE('',*,*,#2989,.T.);
#3867=ORIENTED_EDGE('',*,*,#2990,.T.);
#3868=ORIENTED_EDGE('',*,*,#2989,.F.);
#3869=ORIENTED_EDGE('',*,*,#2988,.T.);
#3870=ORIENTED_EDGE('',*,*,#2985,.T.);
#3871=ORIENTED_EDGE('',*,*,#2990,.F.);
#3872=ORIENTED_EDGE('',*,*,#2987,.F.);
#3873=ORIENTED_EDGE('',*,*,#2991,.F.);
#3874=ORIENTED_EDGE('',*,*,#2992,.T.);
#3875=ORIENTED_EDGE('',*,*,#2993,.T.);
#3876=ORIENTED_EDGE('',*,*,#2992,.F.);
#3877=ORIENTED_EDGE('',*,*,#2994,.F.);
#3878=ORIENTED_EDGE('',*,*,#2995,.T.);
#3879=ORIENTED_EDGE('',*,*,#2996,.T.);
#3880=ORIENTED_EDGE('',*,*,#2995,.F.);
#3881=ORIENTED_EDGE('',*,*,#2994,.T.);
#3882=ORIENTED_EDGE('',*,*,#2991,.T.);
#3883=ORIENTED_EDGE('',*,*,#2996,.F.);
#3884=ORIENTED_EDGE('',*,*,#2993,.F.);
#3885=ORIENTED_EDGE('',*,*,#2997,.F.);
#3886=ORIENTED_EDGE('',*,*,#2998,.T.);
#3887=ORIENTED_EDGE('',*,*,#2999,.T.);
#3888=ORIENTED_EDGE('',*,*,#2998,.F.);
#3889=ORIENTED_EDGE('',*,*,#3000,.F.);
#3890=ORIENTED_EDGE('',*,*,#3001,.T.);
#3891=ORIENTED_EDGE('',*,*,#3002,.T.);
#3892=ORIENTED_EDGE('',*,*,#3001,.F.);
#3893=ORIENTED_EDGE('',*,*,#3000,.T.);
#3894=ORIENTED_EDGE('',*,*,#2997,.T.);
#3895=ORIENTED_EDGE('',*,*,#3002,.F.);
#3896=ORIENTED_EDGE('',*,*,#2999,.F.);
#3897=ORIENTED_EDGE('',*,*,#3003,.F.);
#3898=ORIENTED_EDGE('',*,*,#3004,.T.);
#3899=ORIENTED_EDGE('',*,*,#3005,.F.);
#3900=ORIENTED_EDGE('',*,*,#3004,.F.);
#3901=ORIENTED_EDGE('',*,*,#3006,.F.);
#3902=ORIENTED_EDGE('',*,*,#3007,.T.);
#3903=ORIENTED_EDGE('',*,*,#3008,.F.);
#3904=ORIENTED_EDGE('',*,*,#3007,.F.);
#3905=ORIENTED_EDGE('',*,*,#3009,.F.);
#3906=ORIENTED_EDGE('',*,*,#3010,.T.);
#3907=ORIENTED_EDGE('',*,*,#3011,.T.);
#3908=ORIENTED_EDGE('',*,*,#3010,.F.);
#3909=ORIENTED_EDGE('',*,*,#3011,.F.);
#3910=ORIENTED_EDGE('',*,*,#3012,.F.);
#3911=ORIENTED_EDGE('',*,*,#3013,.F.);
#3912=ORIENTED_EDGE('',*,*,#3014,.T.);
#3913=ORIENTED_EDGE('',*,*,#3015,.T.);
#3914=ORIENTED_EDGE('',*,*,#3014,.F.);
#3915=ORIENTED_EDGE('',*,*,#3015,.F.);
#3916=ORIENTED_EDGE('',*,*,#3016,.F.);
#3917=ORIENTED_EDGE('',*,*,#3012,.T.);
#3918=ORIENTED_EDGE('',*,*,#3017,.T.);
#3919=ORIENTED_EDGE('',*,*,#3018,.F.);
#3920=ORIENTED_EDGE('',*,*,#3017,.F.);
#3921=ORIENTED_EDGE('',*,*,#3016,.T.);
#3922=ORIENTED_EDGE('',*,*,#3019,.T.);
#3923=ORIENTED_EDGE('',*,*,#3020,.F.);
#3924=ORIENTED_EDGE('',*,*,#3019,.F.);
#3925=ORIENTED_EDGE('',*,*,#3021,.T.);
#3926=ORIENTED_EDGE('',*,*,#3022,.T.);
#3927=ORIENTED_EDGE('',*,*,#3023,.F.);
#3928=ORIENTED_EDGE('',*,*,#3024,.F.);
#3929=ORIENTED_EDGE('',*,*,#3025,.T.);
#3930=ORIENTED_EDGE('',*,*,#3024,.T.);
#3931=ORIENTED_EDGE('',*,*,#3026,.F.);
#3932=ORIENTED_EDGE('',*,*,#3027,.F.);
#3933=ORIENTED_EDGE('',*,*,#3028,.T.);
#3934=ORIENTED_EDGE('',*,*,#3027,.T.);
#3935=ORIENTED_EDGE('',*,*,#3029,.F.);
#3936=ORIENTED_EDGE('',*,*,#3030,.F.);
#3937=ORIENTED_EDGE('',*,*,#3031,.T.);
#3938=ORIENTED_EDGE('',*,*,#3030,.T.);
#3939=ORIENTED_EDGE('',*,*,#3032,.F.);
#3940=ORIENTED_EDGE('',*,*,#3022,.F.);
#3941=ORIENTED_EDGE('',*,*,#3032,.T.);
#3942=ORIENTED_EDGE('',*,*,#3029,.T.);
#3943=ORIENTED_EDGE('',*,*,#3026,.T.);
#3944=ORIENTED_EDGE('',*,*,#3023,.T.);
#3945=ORIENTED_EDGE('',*,*,#3005,.T.);
#3946=ORIENTED_EDGE('',*,*,#3008,.T.);
#3947=ORIENTED_EDGE('',*,*,#3018,.T.);
#3948=ORIENTED_EDGE('',*,*,#3020,.T.);
#3949=ORIENTED_EDGE('',*,*,#3031,.F.);
#3950=ORIENTED_EDGE('',*,*,#3021,.F.);
#3951=ORIENTED_EDGE('',*,*,#3025,.F.);
#3952=ORIENTED_EDGE('',*,*,#3028,.F.);
#3953=ORIENTED_EDGE('',*,*,#3003,.T.);
#3954=ORIENTED_EDGE('',*,*,#3006,.T.);
#3955=ORIENTED_EDGE('',*,*,#3009,.T.);
#3956=ORIENTED_EDGE('',*,*,#3013,.T.);
#3957=ORIENTED_EDGE('',*,*,#3033,.F.);
#3958=ORIENTED_EDGE('',*,*,#3034,.F.);
#3959=ORIENTED_EDGE('',*,*,#3035,.T.);
#3960=ORIENTED_EDGE('',*,*,#3033,.T.);
#3961=ORIENTED_EDGE('',*,*,#3035,.F.);
#3962=ORIENTED_EDGE('',*,*,#3036,.F.);
#3963=ORIENTED_EDGE('',*,*,#3037,.T.);
#3964=ORIENTED_EDGE('',*,*,#3034,.T.);
#3965=ORIENTED_EDGE('',*,*,#3037,.F.);
#3966=ORIENTED_EDGE('',*,*,#3038,.F.);
#3967=ORIENTED_EDGE('',*,*,#3039,.T.);
#3968=ORIENTED_EDGE('',*,*,#3036,.T.);
#3969=ORIENTED_EDGE('',*,*,#3039,.F.);
#3970=ORIENTED_EDGE('',*,*,#3038,.T.);
#3971=ORIENTED_EDGE('',*,*,#3040,.F.);
#3972=ORIENTED_EDGE('',*,*,#3041,.F.);
#3973=ORIENTED_EDGE('',*,*,#3042,.T.);
#3974=ORIENTED_EDGE('',*,*,#3040,.T.);
#3975=ORIENTED_EDGE('',*,*,#3042,.F.);
#3976=ORIENTED_EDGE('',*,*,#3043,.F.);
#3977=ORIENTED_EDGE('',*,*,#3044,.T.);
#3978=ORIENTED_EDGE('',*,*,#3041,.T.);
#3979=ORIENTED_EDGE('',*,*,#3044,.F.);
#3980=ORIENTED_EDGE('',*,*,#3045,.F.);
#3981=ORIENTED_EDGE('',*,*,#3046,.T.);
#3982=ORIENTED_EDGE('',*,*,#3043,.T.);
#3983=ORIENTED_EDGE('',*,*,#3046,.F.);
#3984=ORIENTED_EDGE('',*,*,#3045,.T.);
#3985=ORIENTED_EDGE('',*,*,#3047,.T.);
#3986=ORIENTED_EDGE('',*,*,#3048,.T.);
#3987=ORIENTED_EDGE('',*,*,#3049,.T.);
#3988=ORIENTED_EDGE('',*,*,#3050,.F.);
#3989=ORIENTED_EDGE('',*,*,#3051,.T.);
#3990=ORIENTED_EDGE('',*,*,#3052,.T.);
#3991=ORIENTED_EDGE('',*,*,#3053,.T.);
#3992=ORIENTED_EDGE('',*,*,#3048,.F.);
#3993=ORIENTED_EDGE('',*,*,#3054,.T.);
#3994=ORIENTED_EDGE('',*,*,#3055,.T.);
#3995=ORIENTED_EDGE('',*,*,#3056,.T.);
#3996=ORIENTED_EDGE('',*,*,#3052,.F.);
#3997=ORIENTED_EDGE('',*,*,#3057,.T.);
#3998=ORIENTED_EDGE('',*,*,#3058,.T.);
#3999=ORIENTED_EDGE('',*,*,#3059,.T.);
#4000=ORIENTED_EDGE('',*,*,#3055,.F.);
#4001=ORIENTED_EDGE('',*,*,#3060,.T.);
#4002=ORIENTED_EDGE('',*,*,#3061,.T.);
#4003=ORIENTED_EDGE('',*,*,#3062,.T.);
#4004=ORIENTED_EDGE('',*,*,#3058,.F.);
#4005=ORIENTED_EDGE('',*,*,#3063,.T.);
#4006=ORIENTED_EDGE('',*,*,#3050,.T.);
#4007=ORIENTED_EDGE('',*,*,#3064,.T.);
#4008=ORIENTED_EDGE('',*,*,#3061,.F.);
#4009=ORIENTED_EDGE('',*,*,#3063,.F.);
#4010=ORIENTED_EDGE('',*,*,#3060,.F.);
#4011=ORIENTED_EDGE('',*,*,#3057,.F.);
#4012=ORIENTED_EDGE('',*,*,#3054,.F.);
#4013=ORIENTED_EDGE('',*,*,#3051,.F.);
#4014=ORIENTED_EDGE('',*,*,#3047,.F.);
#4015=ORIENTED_EDGE('',*,*,#3064,.F.);
#4016=ORIENTED_EDGE('',*,*,#3049,.F.);
#4017=ORIENTED_EDGE('',*,*,#3053,.F.);
#4018=ORIENTED_EDGE('',*,*,#3056,.F.);
#4019=ORIENTED_EDGE('',*,*,#3059,.F.);
#4020=ORIENTED_EDGE('',*,*,#3062,.F.);
#4021=ORIENTED_EDGE('',*,*,#3065,.F.);
#4022=ORIENTED_EDGE('',*,*,#3066,.T.);
#4023=ORIENTED_EDGE('',*,*,#3067,.F.);
#4024=ORIENTED_EDGE('',*,*,#3066,.F.);
#4025=ORIENTED_EDGE('',*,*,#3065,.T.);
#4026=ORIENTED_EDGE('',*,*,#3068,.F.);
#4027=ORIENTED_EDGE('',*,*,#3069,.T.);
#4028=ORIENTED_EDGE('',*,*,#3070,.T.);
#4029=ORIENTED_EDGE('',*,*,#3071,.T.);
#4030=ORIENTED_EDGE('',*,*,#3072,.T.);
#4031=ORIENTED_EDGE('',*,*,#3073,.T.);
#4032=ORIENTED_EDGE('',*,*,#3074,.T.);
#4033=ORIENTED_EDGE('',*,*,#3075,.T.);
#4034=ORIENTED_EDGE('',*,*,#3076,.F.);
#4035=ORIENTED_EDGE('',*,*,#3077,.F.);
#4036=ORIENTED_EDGE('',*,*,#3078,.F.);
#4037=ORIENTED_EDGE('',*,*,#3079,.F.);
#4038=ORIENTED_EDGE('',*,*,#3080,.F.);
#4039=ORIENTED_EDGE('',*,*,#3081,.F.);
#4040=ORIENTED_EDGE('',*,*,#3082,.F.);
#4041=ORIENTED_EDGE('',*,*,#3077,.T.);
#4042=ORIENTED_EDGE('',*,*,#3083,.T.);
#4043=ORIENTED_EDGE('',*,*,#3074,.F.);
#4044=ORIENTED_EDGE('',*,*,#3084,.F.);
#4045=ORIENTED_EDGE('',*,*,#3078,.T.);
#4046=ORIENTED_EDGE('',*,*,#3084,.T.);
#4047=ORIENTED_EDGE('',*,*,#3073,.F.);
#4048=ORIENTED_EDGE('',*,*,#3085,.F.);
#4049=ORIENTED_EDGE('',*,*,#3079,.T.);
#4050=ORIENTED_EDGE('',*,*,#3085,.T.);
#4051=ORIENTED_EDGE('',*,*,#3072,.F.);
#4052=ORIENTED_EDGE('',*,*,#3086,.F.);
#4053=ORIENTED_EDGE('',*,*,#3080,.T.);
#4054=ORIENTED_EDGE('',*,*,#3086,.T.);
#4055=ORIENTED_EDGE('',*,*,#3071,.F.);
#4056=ORIENTED_EDGE('',*,*,#3087,.F.);
#4057=ORIENTED_EDGE('',*,*,#3081,.T.);
#4058=ORIENTED_EDGE('',*,*,#3087,.T.);
#4059=ORIENTED_EDGE('',*,*,#3070,.F.);
#4060=ORIENTED_EDGE('',*,*,#3088,.F.);
#4061=ORIENTED_EDGE('',*,*,#3076,.T.);
#4062=ORIENTED_EDGE('',*,*,#3088,.T.);
#4063=ORIENTED_EDGE('',*,*,#3069,.F.);
#4064=ORIENTED_EDGE('',*,*,#3083,.F.);
#4065=ORIENTED_EDGE('',*,*,#3089,.F.);
#4066=ORIENTED_EDGE('',*,*,#3067,.T.);
#4067=ORIENTED_EDGE('',*,*,#3089,.T.);
#4068=ORIENTED_EDGE('',*,*,#3090,.T.);
#4069=ORIENTED_EDGE('',*,*,#3091,.F.);
#4070=ORIENTED_EDGE('',*,*,#3090,.F.);
#4071=ORIENTED_EDGE('',*,*,#3092,.F.);
#4072=ORIENTED_EDGE('',*,*,#3091,.T.);
#4073=ORIENTED_EDGE('',*,*,#3075,.F.);
#4074=ORIENTED_EDGE('',*,*,#3093,.T.);
#4075=ORIENTED_EDGE('',*,*,#3092,.T.);
#4076=ORIENTED_EDGE('',*,*,#3093,.F.);
#4077=ORIENTED_EDGE('',*,*,#3094,.F.);
#4078=ORIENTED_EDGE('',*,*,#3095,.T.);
#4079=ORIENTED_EDGE('',*,*,#3082,.T.);
#4080=ORIENTED_EDGE('',*,*,#3095,.F.);
#4081=ORIENTED_EDGE('',*,*,#3094,.T.);
#4082=ORIENTED_EDGE('',*,*,#3096,.F.);
#4083=ORIENTED_EDGE('',*,*,#3096,.T.);
#4084=ORIENTED_EDGE('',*,*,#3097,.T.);
#4085=ORIENTED_EDGE('',*,*,#3068,.T.);
#4086=ORIENTED_EDGE('',*,*,#3097,.F.);
#4087=ORIENTED_EDGE('',*,*,#3098,.F.);
#4088=ORIENTED_EDGE('',*,*,#3099,.T.);
#4089=ORIENTED_EDGE('',*,*,#3100,.F.);
#4090=ORIENTED_EDGE('',*,*,#3101,.T.);
#4091=ORIENTED_EDGE('',*,*,#3098,.T.);
#4092=ORIENTED_EDGE('',*,*,#3101,.F.);
#4093=ORIENTED_EDGE('',*,*,#3100,.T.);
#4094=ORIENTED_EDGE('',*,*,#3102,.F.);
#4095=ORIENTED_EDGE('',*,*,#3103,.F.);
#4096=ORIENTED_EDGE('',*,*,#3104,.T.);
#4097=ORIENTED_EDGE('',*,*,#3102,.T.);
#4098=ORIENTED_EDGE('',*,*,#3104,.F.);
#4099=ORIENTED_EDGE('',*,*,#3103,.T.);
#4100=ORIENTED_EDGE('',*,*,#3105,.F.);
#4101=ORIENTED_EDGE('',*,*,#3105,.T.);
#4102=ORIENTED_EDGE('',*,*,#3106,.T.);
#4103=ORIENTED_EDGE('',*,*,#3099,.F.);
#4104=ORIENTED_EDGE('',*,*,#3106,.F.);
#4105=ORIENTED_EDGE('',*,*,#3107,.F.);
#4106=ORIENTED_EDGE('',*,*,#3108,.T.);
#4107=ORIENTED_EDGE('',*,*,#3107,.T.);
#4108=ORIENTED_EDGE('',*,*,#3108,.F.);
#4109=ORIENTED_EDGE('',*,*,#3109,.F.);
#4110=ORIENTED_EDGE('',*,*,#3110,.T.);
#4111=ORIENTED_EDGE('',*,*,#3111,.T.);
#4112=ORIENTED_EDGE('',*,*,#3110,.F.);
#4113=ORIENTED_EDGE('',*,*,#3111,.F.);
#4114=ORIENTED_EDGE('',*,*,#3112,.F.);
#4115=ORIENTED_EDGE('',*,*,#3109,.T.);
#4116=ORIENTED_EDGE('',*,*,#3113,.F.);
#4117=ORIENTED_EDGE('',*,*,#3113,.T.);
#4118=ORIENTED_EDGE('',*,*,#3114,.T.);
#4119=ORIENTED_EDGE('',*,*,#3115,.T.);
#4120=ORIENTED_EDGE('',*,*,#3114,.F.);
#4121=ORIENTED_EDGE('',*,*,#3116,.F.);
#4122=ORIENTED_EDGE('',*,*,#3117,.T.);
#4123=ORIENTED_EDGE('',*,*,#3112,.T.);
#4124=ORIENTED_EDGE('',*,*,#3117,.F.);
#4125=ORIENTED_EDGE('',*,*,#3118,.F.);
#4126=ORIENTED_EDGE('',*,*,#3119,.T.);
#4127=ORIENTED_EDGE('',*,*,#3120,.T.);
#4128=ORIENTED_EDGE('',*,*,#3119,.F.);
#4129=ORIENTED_EDGE('',*,*,#3118,.T.);
#4130=ORIENTED_EDGE('',*,*,#3116,.T.);
#4131=ORIENTED_EDGE('',*,*,#3120,.F.);
#4132=ORIENTED_EDGE('',*,*,#3115,.F.);
#4133=ORIENTED_EDGE('',*,*,#3121,.F.);
#4134=ORIENTED_EDGE('',*,*,#3122,.T.);
#4135=ORIENTED_EDGE('',*,*,#3121,.T.);
#4136=ORIENTED_EDGE('',*,*,#3122,.F.);
#4137=ORIENTED_EDGE('',*,*,#3123,.F.);
#4138=ORIENTED_EDGE('',*,*,#3124,.T.);
#4139=ORIENTED_EDGE('',*,*,#3125,.T.);
#4140=ORIENTED_EDGE('',*,*,#3124,.F.);
#4141=ORIENTED_EDGE('',*,*,#3123,.T.);
#4142=ORIENTED_EDGE('',*,*,#3125,.F.);
#4143=ORIENTED_EDGE('',*,*,#3126,.T.);
#4144=ORIENTED_EDGE('',*,*,#3127,.T.);
#4145=ORIENTED_EDGE('',*,*,#3128,.T.);
#4146=ORIENTED_EDGE('',*,*,#3127,.F.);
#4147=ORIENTED_EDGE('',*,*,#3128,.F.);
#4148=ORIENTED_EDGE('',*,*,#3129,.T.);
#4149=ORIENTED_EDGE('',*,*,#3130,.T.);
#4150=ORIENTED_EDGE('',*,*,#3129,.F.);
#4151=ORIENTED_EDGE('',*,*,#3131,.T.);
#4152=ORIENTED_EDGE('',*,*,#3126,.F.);
#4153=ORIENTED_EDGE('',*,*,#3131,.F.);
#4154=ORIENTED_EDGE('',*,*,#3132,.T.);
#4155=ORIENTED_EDGE('',*,*,#3133,.T.);
#4156=ORIENTED_EDGE('',*,*,#3132,.F.);
#4157=ORIENTED_EDGE('',*,*,#3133,.F.);
#4158=ORIENTED_EDGE('',*,*,#3130,.F.);
#4159=ORIENTED_EDGE('',*,*,#3134,.F.);
#4160=ORIENTED_EDGE('',*,*,#3135,.F.);
#4161=ORIENTED_EDGE('',*,*,#3136,.T.);
#4162=ORIENTED_EDGE('',*,*,#3137,.F.);
#4163=ORIENTED_EDGE('',*,*,#3136,.F.);
#4164=ORIENTED_EDGE('',*,*,#3138,.F.);
#4165=ORIENTED_EDGE('',*,*,#3139,.F.);
#4166=ORIENTED_EDGE('',*,*,#3140,.F.);
#4167=ORIENTED_EDGE('',*,*,#3141,.F.);
#4168=ORIENTED_EDGE('',*,*,#3142,.F.);
#4169=ORIENTED_EDGE('',*,*,#3143,.T.);
#4170=ORIENTED_EDGE('',*,*,#3144,.F.);
#4171=ORIENTED_EDGE('',*,*,#3145,.F.);
#4172=ORIENTED_EDGE('',*,*,#3146,.F.);
#4173=ORIENTED_EDGE('',*,*,#3147,.F.);
#4174=ORIENTED_EDGE('',*,*,#3148,.F.);
#4175=ORIENTED_EDGE('',*,*,#3149,.F.);
#4176=ORIENTED_EDGE('',*,*,#3143,.F.);
#4177=ORIENTED_EDGE('',*,*,#3139,.T.);
#4178=ORIENTED_EDGE('',*,*,#3150,.T.);
#4179=ORIENTED_EDGE('',*,*,#3148,.T.);
#4180=ORIENTED_EDGE('',*,*,#3151,.F.);
#4181=ORIENTED_EDGE('',*,*,#3138,.T.);
#4182=ORIENTED_EDGE('',*,*,#3152,.T.);
#4183=ORIENTED_EDGE('',*,*,#3149,.T.);
#4184=ORIENTED_EDGE('',*,*,#3150,.F.);
#4185=ORIENTED_EDGE('',*,*,#3135,.T.);
#4186=ORIENTED_EDGE('',*,*,#3153,.T.);
#4187=ORIENTED_EDGE('',*,*,#3144,.T.);
#4188=ORIENTED_EDGE('',*,*,#3152,.F.);
#4189=ORIENTED_EDGE('',*,*,#3154,.F.);
#4190=ORIENTED_EDGE('',*,*,#3155,.T.);
#4191=ORIENTED_EDGE('',*,*,#3156,.T.);
#4192=ORIENTED_EDGE('',*,*,#3155,.F.);
#4193=ORIENTED_EDGE('',*,*,#3134,.T.);
#4194=ORIENTED_EDGE('',*,*,#3157,.T.);
#4195=ORIENTED_EDGE('',*,*,#3145,.T.);
#4196=ORIENTED_EDGE('',*,*,#3153,.F.);
#4197=ORIENTED_EDGE('',*,*,#3140,.T.);
#4198=ORIENTED_EDGE('',*,*,#3151,.T.);
#4199=ORIENTED_EDGE('',*,*,#3147,.T.);
#4200=ORIENTED_EDGE('',*,*,#3158,.F.);
#4201=ORIENTED_EDGE('',*,*,#3141,.T.);
#4202=ORIENTED_EDGE('',*,*,#3158,.T.);
#4203=ORIENTED_EDGE('',*,*,#3146,.T.);
#4204=ORIENTED_EDGE('',*,*,#3157,.F.);
#4205=ORIENTED_EDGE('',*,*,#3142,.T.);
#4206=ORIENTED_EDGE('',*,*,#3154,.T.);
#4207=ORIENTED_EDGE('',*,*,#3137,.T.);
#4208=ORIENTED_EDGE('',*,*,#3156,.F.);
#4209=ORIENTED_EDGE('',*,*,#3159,.F.);
#4210=ORIENTED_EDGE('',*,*,#3160,.T.);
#4211=ORIENTED_EDGE('',*,*,#3161,.F.);
#4212=ORIENTED_EDGE('',*,*,#3160,.F.);
#4213=ORIENTED_EDGE('',*,*,#3159,.T.);
#4214=ORIENTED_EDGE('',*,*,#3162,.F.);
#4215=ORIENTED_EDGE('',*,*,#3163,.F.);
#4216=ORIENTED_EDGE('',*,*,#3164,.T.);
#4217=ORIENTED_EDGE('',*,*,#3165,.T.);
#4218=ORIENTED_EDGE('',*,*,#3164,.F.);
#4219=ORIENTED_EDGE('',*,*,#3166,.F.);
#4220=ORIENTED_EDGE('',*,*,#3165,.F.);
#4221=ORIENTED_EDGE('',*,*,#3167,.F.);
#4222=ORIENTED_EDGE('',*,*,#3163,.T.);
#4223=ORIENTED_EDGE('',*,*,#3167,.T.);
#4224=ORIENTED_EDGE('',*,*,#3168,.T.);
#4225=ORIENTED_EDGE('',*,*,#3169,.T.);
#4226=ORIENTED_EDGE('',*,*,#3168,.F.);
#4227=ORIENTED_EDGE('',*,*,#3162,.T.);
#4228=ORIENTED_EDGE('',*,*,#3170,.T.);
#4229=ORIENTED_EDGE('',*,*,#3171,.T.);
#4230=ORIENTED_EDGE('',*,*,#3170,.F.);
#4231=ORIENTED_EDGE('',*,*,#3172,.F.);
#4232=ORIENTED_EDGE('',*,*,#3173,.T.);
#4233=ORIENTED_EDGE('',*,*,#3166,.T.);
#4234=ORIENTED_EDGE('',*,*,#3173,.F.);
#4235=ORIENTED_EDGE('',*,*,#3172,.T.);
#4236=ORIENTED_EDGE('',*,*,#3161,.T.);
#4237=ORIENTED_EDGE('',*,*,#3169,.F.);
#4238=ORIENTED_EDGE('',*,*,#3171,.F.);
#4239=ORIENTED_EDGE('',*,*,#3174,.F.);
#4240=ORIENTED_EDGE('',*,*,#3175,.T.);
#4241=ORIENTED_EDGE('',*,*,#3174,.T.);
#4242=ORIENTED_EDGE('',*,*,#3175,.F.);
#4243=ORIENTED_EDGE('',*,*,#3176,.F.);
#4244=ORIENTED_EDGE('',*,*,#3177,.T.);
#4245=ORIENTED_EDGE('',*,*,#3178,.F.);
#4246=ORIENTED_EDGE('',*,*,#3177,.F.);
#4247=ORIENTED_EDGE('',*,*,#3176,.T.);
#4248=ORIENTED_EDGE('',*,*,#3179,.F.);
#4249=ORIENTED_EDGE('',*,*,#3180,.T.);
#4250=ORIENTED_EDGE('',*,*,#3181,.T.);
#4251=ORIENTED_EDGE('',*,*,#3180,.F.);
#4252=ORIENTED_EDGE('',*,*,#3179,.T.);
#4253=ORIENTED_EDGE('',*,*,#3178,.T.);
#4254=ORIENTED_EDGE('',*,*,#3181,.F.);
#4255=ORIENTED_EDGE('',*,*,#3182,.F.);
#4256=ORIENTED_EDGE('',*,*,#3183,.F.);
#4257=ORIENTED_EDGE('',*,*,#3184,.T.);
#4258=ORIENTED_EDGE('',*,*,#3182,.T.);
#4259=ORIENTED_EDGE('',*,*,#3184,.F.);
#4260=ORIENTED_EDGE('',*,*,#3185,.F.);
#4261=ORIENTED_EDGE('',*,*,#3186,.T.);
#4262=ORIENTED_EDGE('',*,*,#3183,.T.);
#4263=ORIENTED_EDGE('',*,*,#3186,.F.);
#4264=ORIENTED_EDGE('',*,*,#3187,.F.);
#4265=ORIENTED_EDGE('',*,*,#3188,.T.);
#4266=ORIENTED_EDGE('',*,*,#3185,.T.);
#4267=ORIENTED_EDGE('',*,*,#3188,.F.);
#4268=ORIENTED_EDGE('',*,*,#3187,.T.);
#4269=ORIENTED_EDGE('',*,*,#3189,.F.);
#4270=ORIENTED_EDGE('',*,*,#3190,.F.);
#4271=ORIENTED_EDGE('',*,*,#3191,.T.);
#4272=ORIENTED_EDGE('',*,*,#3189,.T.);
#4273=ORIENTED_EDGE('',*,*,#3191,.F.);
#4274=ORIENTED_EDGE('',*,*,#3192,.F.);
#4275=ORIENTED_EDGE('',*,*,#3193,.T.);
#4276=ORIENTED_EDGE('',*,*,#3190,.T.);
#4277=ORIENTED_EDGE('',*,*,#3193,.F.);
#4278=ORIENTED_EDGE('',*,*,#3194,.F.);
#4279=ORIENTED_EDGE('',*,*,#3195,.T.);
#4280=ORIENTED_EDGE('',*,*,#3192,.T.);
#4281=ORIENTED_EDGE('',*,*,#3195,.F.);
#4282=ORIENTED_EDGE('',*,*,#3194,.T.);
#4283=ORIENTED_EDGE('',*,*,#3196,.T.);
#4284=ORIENTED_EDGE('',*,*,#3197,.T.);
#4285=ORIENTED_EDGE('',*,*,#3198,.T.);
#4286=ORIENTED_EDGE('',*,*,#3199,.F.);
#4287=ORIENTED_EDGE('',*,*,#3200,.T.);
#4288=ORIENTED_EDGE('',*,*,#3201,.T.);
#4289=ORIENTED_EDGE('',*,*,#3202,.T.);
#4290=ORIENTED_EDGE('',*,*,#3197,.F.);
#4291=ORIENTED_EDGE('',*,*,#3203,.T.);
#4292=ORIENTED_EDGE('',*,*,#3204,.T.);
#4293=ORIENTED_EDGE('',*,*,#3205,.T.);
#4294=ORIENTED_EDGE('',*,*,#3201,.F.);
#4295=ORIENTED_EDGE('',*,*,#3206,.T.);
#4296=ORIENTED_EDGE('',*,*,#3207,.T.);
#4297=ORIENTED_EDGE('',*,*,#3208,.T.);
#4298=ORIENTED_EDGE('',*,*,#3204,.F.);
#4299=ORIENTED_EDGE('',*,*,#3209,.T.);
#4300=ORIENTED_EDGE('',*,*,#3210,.T.);
#4301=ORIENTED_EDGE('',*,*,#3211,.T.);
#4302=ORIENTED_EDGE('',*,*,#3207,.F.);
#4303=ORIENTED_EDGE('',*,*,#3212,.T.);
#4304=ORIENTED_EDGE('',*,*,#3199,.T.);
#4305=ORIENTED_EDGE('',*,*,#3213,.T.);
#4306=ORIENTED_EDGE('',*,*,#3210,.F.);
#4307=ORIENTED_EDGE('',*,*,#3212,.F.);
#4308=ORIENTED_EDGE('',*,*,#3209,.F.);
#4309=ORIENTED_EDGE('',*,*,#3206,.F.);
#4310=ORIENTED_EDGE('',*,*,#3203,.F.);
#4311=ORIENTED_EDGE('',*,*,#3200,.F.);
#4312=ORIENTED_EDGE('',*,*,#3196,.F.);
#4313=ORIENTED_EDGE('',*,*,#3213,.F.);
#4314=ORIENTED_EDGE('',*,*,#3198,.F.);
#4315=ORIENTED_EDGE('',*,*,#3202,.F.);
#4316=ORIENTED_EDGE('',*,*,#3205,.F.);
#4317=ORIENTED_EDGE('',*,*,#3208,.F.);
#4318=ORIENTED_EDGE('',*,*,#3211,.F.);
#4319=ORIENTED_EDGE('',*,*,#3214,.F.);
#4320=ORIENTED_EDGE('',*,*,#3215,.T.);
#4321=ORIENTED_EDGE('',*,*,#3216,.F.);
#4322=ORIENTED_EDGE('',*,*,#3215,.F.);
#4323=ORIENTED_EDGE('',*,*,#3217,.F.);
#4324=ORIENTED_EDGE('',*,*,#3218,.T.);
#4325=ORIENTED_EDGE('',*,*,#3219,.F.);
#4326=ORIENTED_EDGE('',*,*,#3218,.F.);
#4327=ORIENTED_EDGE('',*,*,#3220,.F.);
#4328=ORIENTED_EDGE('',*,*,#3221,.T.);
#4329=ORIENTED_EDGE('',*,*,#3222,.F.);
#4330=ORIENTED_EDGE('',*,*,#3223,.F.);
#4331=ORIENTED_EDGE('',*,*,#3224,.T.);
#4332=ORIENTED_EDGE('',*,*,#3225,.F.);
#4333=ORIENTED_EDGE('',*,*,#3224,.F.);
#4334=ORIENTED_EDGE('',*,*,#3226,.F.);
#4335=ORIENTED_EDGE('',*,*,#3227,.F.);
#4336=ORIENTED_EDGE('',*,*,#3221,.F.);
#4337=ORIENTED_EDGE('',*,*,#3228,.F.);
#4338=ORIENTED_EDGE('',*,*,#3226,.T.);
#4339=ORIENTED_EDGE('',*,*,#3223,.T.);
#4340=ORIENTED_EDGE('',*,*,#3229,.F.);
#4341=ORIENTED_EDGE('',*,*,#3230,.T.);
#4342=ORIENTED_EDGE('',*,*,#3231,.F.);
#4343=ORIENTED_EDGE('',*,*,#3230,.F.);
#4344=ORIENTED_EDGE('',*,*,#3227,.T.);
#4345=ORIENTED_EDGE('',*,*,#3228,.T.);
#4346=ORIENTED_EDGE('',*,*,#3222,.T.);
#4347=ORIENTED_EDGE('',*,*,#3220,.T.);
#4348=ORIENTED_EDGE('',*,*,#3232,.F.);
#4349=ORIENTED_EDGE('',*,*,#3233,.F.);
#4350=ORIENTED_EDGE('',*,*,#3234,.F.);
#4351=ORIENTED_EDGE('',*,*,#3235,.F.);
#4352=ORIENTED_EDGE('',*,*,#3217,.T.);
#4353=ORIENTED_EDGE('',*,*,#3236,.F.);
#4354=ORIENTED_EDGE('',*,*,#3237,.F.);
#4355=ORIENTED_EDGE('',*,*,#3238,.F.);
#4356=ORIENTED_EDGE('',*,*,#3233,.T.);
#4357=ORIENTED_EDGE('',*,*,#3229,.T.);
#4358=ORIENTED_EDGE('',*,*,#3239,.F.);
#4359=ORIENTED_EDGE('',*,*,#3240,.F.);
#4360=ORIENTED_EDGE('',*,*,#3241,.F.);
#4361=ORIENTED_EDGE('',*,*,#3237,.T.);
#4362=ORIENTED_EDGE('',*,*,#3216,.T.);
#4363=ORIENTED_EDGE('',*,*,#3234,.T.);
#4364=ORIENTED_EDGE('',*,*,#3238,.T.);
#4365=ORIENTED_EDGE('',*,*,#3241,.T.);
#4366=ORIENTED_EDGE('',*,*,#3242,.F.);
#4367=ORIENTED_EDGE('',*,*,#3243,.F.);
#4368=ORIENTED_EDGE('',*,*,#3244,.F.);
#4369=ORIENTED_EDGE('',*,*,#3245,.F.);
#4370=ORIENTED_EDGE('',*,*,#3246,.F.);
#4371=ORIENTED_EDGE('',*,*,#3240,.T.);
#4372=ORIENTED_EDGE('',*,*,#3247,.F.);
#4373=ORIENTED_EDGE('',*,*,#3248,.F.);
#4374=ORIENTED_EDGE('',*,*,#3242,.T.);
#4375=ORIENTED_EDGE('',*,*,#3235,.T.);
#4376=ORIENTED_EDGE('',*,*,#3246,.T.);
#4377=ORIENTED_EDGE('',*,*,#3249,.T.);
#4378=ORIENTED_EDGE('',*,*,#3250,.F.);
#4379=ORIENTED_EDGE('',*,*,#3244,.T.);
#4380=ORIENTED_EDGE('',*,*,#3251,.T.);
#4381=ORIENTED_EDGE('',*,*,#3252,.F.);
#4382=ORIENTED_EDGE('',*,*,#3253,.F.);
#4383=ORIENTED_EDGE('',*,*,#3231,.T.);
#4384=ORIENTED_EDGE('',*,*,#3245,.T.);
#4385=ORIENTED_EDGE('',*,*,#3253,.T.);
#4386=ORIENTED_EDGE('',*,*,#3254,.F.);
#4387=ORIENTED_EDGE('',*,*,#3249,.F.);
#4388=ORIENTED_EDGE('',*,*,#3219,.T.);
#4389=ORIENTED_EDGE('',*,*,#3243,.T.);
#4390=ORIENTED_EDGE('',*,*,#3248,.T.);
#4391=ORIENTED_EDGE('',*,*,#3255,.F.);
#4392=ORIENTED_EDGE('',*,*,#3251,.F.);
#4393=ORIENTED_EDGE('',*,*,#3214,.T.);
#4394=ORIENTED_EDGE('',*,*,#3232,.T.);
#4395=ORIENTED_EDGE('',*,*,#3250,.T.);
#4396=ORIENTED_EDGE('',*,*,#3254,.T.);
#4397=ORIENTED_EDGE('',*,*,#3252,.T.);
#4398=ORIENTED_EDGE('',*,*,#3255,.T.);
#4399=ORIENTED_EDGE('',*,*,#3247,.T.);
#4400=ORIENTED_EDGE('',*,*,#3239,.T.);
#4401=ORIENTED_EDGE('',*,*,#3236,.T.);
#4402=ORIENTED_EDGE('',*,*,#3225,.T.);
#4403=ORIENTED_EDGE('',*,*,#3256,.F.);
#4404=ORIENTED_EDGE('',*,*,#3257,.T.);
#4405=ORIENTED_EDGE('',*,*,#3258,.T.);
#4406=ORIENTED_EDGE('',*,*,#3259,.F.);
#4407=ORIENTED_EDGE('',*,*,#3260,.F.);
#4408=ORIENTED_EDGE('',*,*,#3261,.T.);
#4409=ORIENTED_EDGE('',*,*,#3262,.T.);
#4410=ORIENTED_EDGE('',*,*,#3257,.F.);
#4411=ORIENTED_EDGE('',*,*,#3263,.F.);
#4412=ORIENTED_EDGE('',*,*,#3264,.T.);
#4413=ORIENTED_EDGE('',*,*,#3265,.T.);
#4414=ORIENTED_EDGE('',*,*,#3261,.F.);
#4415=ORIENTED_EDGE('',*,*,#3266,.F.);
#4416=ORIENTED_EDGE('',*,*,#3267,.T.);
#4417=ORIENTED_EDGE('',*,*,#3268,.T.);
#4418=ORIENTED_EDGE('',*,*,#3264,.F.);
#4419=ORIENTED_EDGE('',*,*,#3269,.F.);
#4420=ORIENTED_EDGE('',*,*,#3270,.T.);
#4421=ORIENTED_EDGE('',*,*,#3271,.T.);
#4422=ORIENTED_EDGE('',*,*,#3267,.F.);
#4423=ORIENTED_EDGE('',*,*,#3272,.F.);
#4424=ORIENTED_EDGE('',*,*,#3259,.T.);
#4425=ORIENTED_EDGE('',*,*,#3273,.T.);
#4426=ORIENTED_EDGE('',*,*,#3270,.F.);
#4427=ORIENTED_EDGE('',*,*,#3273,.F.);
#4428=ORIENTED_EDGE('',*,*,#3258,.F.);
#4429=ORIENTED_EDGE('',*,*,#3262,.F.);
#4430=ORIENTED_EDGE('',*,*,#3265,.F.);
#4431=ORIENTED_EDGE('',*,*,#3268,.F.);
#4432=ORIENTED_EDGE('',*,*,#3271,.F.);
#4433=ORIENTED_EDGE('',*,*,#3274,.F.);
#4434=ORIENTED_EDGE('',*,*,#3256,.T.);
#4435=ORIENTED_EDGE('',*,*,#3272,.T.);
#4436=ORIENTED_EDGE('',*,*,#3269,.T.);
#4437=ORIENTED_EDGE('',*,*,#3266,.T.);
#4438=ORIENTED_EDGE('',*,*,#3263,.T.);
#4439=ORIENTED_EDGE('',*,*,#3260,.T.);
#4440=ORIENTED_EDGE('',*,*,#3275,.F.);
#4441=ORIENTED_EDGE('',*,*,#3276,.T.);
#4442=ORIENTED_EDGE('',*,*,#3274,.T.);
#4443=ORIENTED_EDGE('',*,*,#3276,.F.);
#4444=ORIENTED_EDGE('',*,*,#3277,.F.);
#4445=ORIENTED_EDGE('',*,*,#3278,.T.);
#4446=ORIENTED_EDGE('',*,*,#3275,.T.);
#4447=ORIENTED_EDGE('',*,*,#3278,.F.);
#4448=ORIENTED_EDGE('',*,*,#3279,.F.);
#4449=ORIENTED_EDGE('',*,*,#3280,.T.);
#4450=ORIENTED_EDGE('',*,*,#3277,.T.);
#4451=ORIENTED_EDGE('',*,*,#3280,.F.);
#4452=ORIENTED_EDGE('',*,*,#3279,.T.);
#4453=ORIENTED_EDGE('',*,*,#3281,.F.);
#4454=ORIENTED_EDGE('',*,*,#3282,.T.);
#4455=ORIENTED_EDGE('',*,*,#3283,.F.);
#4456=ORIENTED_EDGE('',*,*,#3282,.F.);
#4457=ORIENTED_EDGE('',*,*,#3284,.F.);
#4458=ORIENTED_EDGE('',*,*,#3285,.F.);
#4459=ORIENTED_EDGE('',*,*,#3286,.F.);
#4460=ORIENTED_EDGE('',*,*,#3287,.F.);
#4461=ORIENTED_EDGE('',*,*,#3288,.T.);
#4462=ORIENTED_EDGE('',*,*,#3286,.T.);
#4463=ORIENTED_EDGE('',*,*,#3288,.F.);
#4464=ORIENTED_EDGE('',*,*,#3289,.F.);
#4465=ORIENTED_EDGE('',*,*,#3290,.T.);
#4466=ORIENTED_EDGE('',*,*,#3287,.T.);
#4467=ORIENTED_EDGE('',*,*,#3290,.F.);
#4468=ORIENTED_EDGE('',*,*,#3289,.T.);
#4469=ORIENTED_EDGE('',*,*,#3291,.F.);
#4470=ORIENTED_EDGE('',*,*,#3292,.F.);
#4471=ORIENTED_EDGE('',*,*,#3293,.T.);
#4472=ORIENTED_EDGE('',*,*,#3285,.T.);
#4473=ORIENTED_EDGE('',*,*,#3294,.T.);
#4474=ORIENTED_EDGE('',*,*,#3291,.T.);
#4475=ORIENTED_EDGE('',*,*,#3294,.F.);
#4476=ORIENTED_EDGE('',*,*,#3284,.T.);
#4477=ORIENTED_EDGE('',*,*,#3281,.T.);
#4478=ORIENTED_EDGE('',*,*,#3293,.F.);
#4479=ORIENTED_EDGE('',*,*,#3283,.T.);
#4480=ORIENTED_EDGE('',*,*,#3295,.F.);
#4481=ORIENTED_EDGE('',*,*,#3296,.T.);
#4482=ORIENTED_EDGE('',*,*,#3292,.T.);
#4483=ORIENTED_EDGE('',*,*,#3296,.F.);
#4484=ORIENTED_EDGE('',*,*,#3295,.T.);
#4485=ORIENTED_EDGE('',*,*,#3297,.F.);
#4486=ORIENTED_EDGE('',*,*,#3298,.T.);
#4487=ORIENTED_EDGE('',*,*,#3299,.T.);
#4488=ORIENTED_EDGE('',*,*,#3298,.F.);
#4489=ORIENTED_EDGE('',*,*,#3300,.F.);
#4490=ORIENTED_EDGE('',*,*,#3301,.T.);
#4491=ORIENTED_EDGE('',*,*,#3302,.T.);
#4492=ORIENTED_EDGE('',*,*,#3301,.F.);
#4493=ORIENTED_EDGE('',*,*,#3300,.T.);
#4494=ORIENTED_EDGE('',*,*,#3297,.T.);
#4495=ORIENTED_EDGE('',*,*,#3302,.F.);
#4496=ORIENTED_EDGE('',*,*,#3299,.F.);
#4497=ORIENTED_EDGE('',*,*,#3303,.F.);
#4498=ORIENTED_EDGE('',*,*,#3304,.T.);
#4499=ORIENTED_EDGE('',*,*,#3303,.T.);
#4500=ORIENTED_EDGE('',*,*,#3304,.F.);
#4501=ORIENTED_EDGE('',*,*,#3305,.F.);
#4502=ORIENTED_EDGE('',*,*,#3306,.F.);
#4503=ORIENTED_EDGE('',*,*,#3307,.T.);
#4504=ORIENTED_EDGE('',*,*,#3308,.F.);
#4505=ORIENTED_EDGE('',*,*,#3308,.T.);
#4506=ORIENTED_EDGE('',*,*,#3309,.T.);
#4507=ORIENTED_EDGE('',*,*,#3310,.F.);
#4508=ORIENTED_EDGE('',*,*,#3311,.F.);
#4509=ORIENTED_EDGE('',*,*,#3307,.F.);
#4510=ORIENTED_EDGE('',*,*,#3311,.T.);
#4511=ORIENTED_EDGE('',*,*,#3312,.F.);
#4512=ORIENTED_EDGE('',*,*,#3313,.T.);
#4513=ORIENTED_EDGE('',*,*,#3306,.T.);
#4514=ORIENTED_EDGE('',*,*,#3305,.T.);
#4515=ORIENTED_EDGE('',*,*,#3313,.F.);
#4516=ORIENTED_EDGE('',*,*,#3314,.F.);
#4517=ORIENTED_EDGE('',*,*,#3309,.F.);
#4518=ORIENTED_EDGE('',*,*,#3314,.T.);
#4519=ORIENTED_EDGE('',*,*,#3312,.T.);
#4520=ORIENTED_EDGE('',*,*,#3310,.T.);
#4521=CYLINDRICAL_SURFACE('',#5266,0.21);
#4522=CYLINDRICAL_SURFACE('',#5270,0.21);
#4523=CYLINDRICAL_SURFACE('',#5278,0.2);
#4524=CYLINDRICAL_SURFACE('',#5281,0.2);
#4525=CYLINDRICAL_SURFACE('',#5288,0.2);
#4526=CYLINDRICAL_SURFACE('',#5299,0.2);
#4527=CYLINDRICAL_SURFACE('',#5300,0.2);
#4528=CYLINDRICAL_SURFACE('',#5302,0.2);
#4529=CYLINDRICAL_SURFACE('',#5304,1.);
#4530=CYLINDRICAL_SURFACE('',#5309,0.685);
#4531=CYLINDRICAL_SURFACE('',#5313,0.275);
#4532=CYLINDRICAL_SURFACE('',#5316,0.275);
#4533=CYLINDRICAL_SURFACE('',#5319,0.275);
#4534=CYLINDRICAL_SURFACE('',#5322,0.275);
#4535=CYLINDRICAL_SURFACE('',#5325,0.6);
#4536=CYLINDRICAL_SURFACE('',#5336,0.515);
#4537=CYLINDRICAL_SURFACE('',#5343,0.4);
#4538=CYLINDRICAL_SURFACE('',#5345,0.49);
#4539=CYLINDRICAL_SURFACE('',#5352,0.25);
#4540=CYLINDRICAL_SURFACE('',#5353,0.25);
#4541=CYLINDRICAL_SURFACE('',#5374,0.2);
#4542=CYLINDRICAL_SURFACE('',#5376,0.685);
#4543=CYLINDRICAL_SURFACE('',#5384,0.3);
#4544=CYLINDRICAL_SURFACE('',#5388,0.6);
#4545=CYLINDRICAL_SURFACE('',#5392,0.21);
#4546=CYLINDRICAL_SURFACE('',#5396,0.21);
#4547=CYLINDRICAL_SURFACE('',#5406,0.2);
#4548=CYLINDRICAL_SURFACE('',#5413,0.2);
#4549=CYLINDRICAL_SURFACE('',#5416,0.2);
#4550=CYLINDRICAL_SURFACE('',#5427,0.2);
#4551=CYLINDRICAL_SURFACE('',#5428,0.2);
#4552=CYLINDRICAL_SURFACE('',#5429,0.2);
#4553=CYLINDRICAL_SURFACE('',#5434,0.685);
#4554=CYLINDRICAL_SURFACE('',#5438,0.275);
#4555=CYLINDRICAL_SURFACE('',#5441,0.275);
#4556=CYLINDRICAL_SURFACE('',#5444,0.275);
#4557=CYLINDRICAL_SURFACE('',#5447,0.275);
#4558=CYLINDRICAL_SURFACE('',#5450,1.);
#4559=CYLINDRICAL_SURFACE('',#5459,0.515);
#4560=CYLINDRICAL_SURFACE('',#5466,0.4);
#4561=CYLINDRICAL_SURFACE('',#5468,0.49);
#4562=CYLINDRICAL_SURFACE('',#5475,0.25);
#4563=CYLINDRICAL_SURFACE('',#5476,0.25);
#4564=CYLINDRICAL_SURFACE('',#5497,0.2);
#4565=CYLINDRICAL_SURFACE('',#5499,0.685);
#4566=CYLINDRICAL_SURFACE('',#5507,0.3);
#4567=CYLINDRICAL_SURFACE('',#5511,0.6);
#4568=CYLINDRICAL_SURFACE('',#5515,1.);
#4569=CYLINDRICAL_SURFACE('',#5518,1.6);
#4570=CYLINDRICAL_SURFACE('',#5524,1.);
#4571=CYLINDRICAL_SURFACE('',#5527,1.6);
#4572=CYLINDRICAL_SURFACE('',#5533,1.);
#4573=CYLINDRICAL_SURFACE('',#5536,1.6);
#4574=CYLINDRICAL_SURFACE('',#5542,0.275);
#4575=CYLINDRICAL_SURFACE('',#5545,0.275);
#4576=CYLINDRICAL_SURFACE('',#5548,0.5);
#4577=CYLINDRICAL_SURFACE('',#5553,0.5);
#4578=CYLINDRICAL_SURFACE('',#5558,0.275);
#4579=CYLINDRICAL_SURFACE('',#5560,0.275);
#4580=CYLINDRICAL_SURFACE('',#5573,0.425);
#4581=CYLINDRICAL_SURFACE('',#5581,0.24505);
#4582=CYLINDRICAL_SURFACE('',#5596,0.43);
#4583=CYLINDRICAL_SURFACE('',#5613,0.46);
#4584=CYLINDRICAL_SURFACE('',#5617,0.525);
#4585=CYLINDRICAL_SURFACE('',#5618,0.515);
#4586=CYLINDRICAL_SURFACE('',#5622,0.2);
#4587=CYLINDRICAL_SURFACE('',#5627,0.475);
#4588=CYLINDRICAL_SURFACE('',#5631,0.355);
#4589=CYLINDRICAL_SURFACE('',#5635,0.31);
#4590=CYLINDRICAL_SURFACE('',#5643,0.51);
#4591=CYLINDRICAL_SURFACE('',#5650,0.405);
#4592=CYLINDRICAL_SURFACE('',#5652,0.405);
#4593=CYLINDRICAL_SURFACE('',#5654,0.6);
#4594=CYLINDRICAL_SURFACE('',#5664,0.25);
#4595=CYLINDRICAL_SURFACE('',#5673,0.265);
#4596=CYLINDRICAL_SURFACE('',#5677,0.5);
#4597=CYLINDRICAL_SURFACE('',#5688,0.2117);
#4598=CYLINDRICAL_SURFACE('',#5739,0.4);
#4599=CYLINDRICAL_SURFACE('',#5744,0.9);
#4600=CYLINDRICAL_SURFACE('',#5751,0.99);
#4601=CYLINDRICAL_SURFACE('',#5753,0.225);
#4602=CYLINDRICAL_SURFACE('',#5755,0.99);
#4603=CYLINDRICAL_SURFACE('',#5764,0.165);
#4604=CYLINDRICAL_SURFACE('',#5768,0.4);
#4605=CYLINDRICAL_SURFACE('',#5778,0.35);
#4606=CYLINDRICAL_SURFACE('',#5786,0.1954);
#4607=CYLINDRICAL_SURFACE('',#5800,0.305);
#4608=CYLINDRICAL_SURFACE('',#5803,0.305);
#4609=CYLINDRICAL_SURFACE('',#5808,0.165);
#4610=CYLINDRICAL_SURFACE('',#5813,0.4);
#4611=CYLINDRICAL_SURFACE('',#5838,0.1954);
#4612=CYLINDRICAL_SURFACE('',#5844,0.08);
#4613=CYLINDRICAL_SURFACE('',#5849,0.5);
#4614=CYLINDRICAL_SURFACE('',#5853,0.3);
#4615=CYLINDRICAL_SURFACE('',#5859,0.32);
#4616=CYLINDRICAL_SURFACE('',#5862,0.6);
#4617=CYLINDRICAL_SURFACE('',#5874,0.08);
#4618=ADVANCED_FACE('',(#695),#4521,.F.);
#4619=ADVANCED_FACE('',(#696),#509,.F.);
#4620=ADVANCED_FACE('',(#697),#4522,.F.);
#4621=ADVANCED_FACE('',(#698),#510,.F.);
#4622=ADVANCED_FACE('',(#699),#511,.T.);
#4623=ADVANCED_FACE('',(#700),#512,.T.);
#4624=ADVANCED_FACE('',(#701),#4523,.F.);
#4625=ADVANCED_FACE('',(#702),#4524,.F.);
#4626=ADVANCED_FACE('',(#703),#4525,.F.);
#4627=ADVANCED_FACE('',(#704),#513,.F.);
#4628=ADVANCED_FACE('',(#705),#514,.T.);
#4629=ADVANCED_FACE('',(#706),#515,.T.);
#4630=ADVANCED_FACE('',(#707),#516,.T.);
#4631=ADVANCED_FACE('',(#708),#4526,.F.);
#4632=ADVANCED_FACE('',(#709),#4527,.F.);
#4633=ADVANCED_FACE('',(#710),#4528,.F.);
#4634=ADVANCED_FACE('',(#711),#4529,.F.);
#4635=ADVANCED_FACE('',(#712),#517,.T.);
#4636=ADVANCED_FACE('',(#713),#4530,.F.);
#4637=ADVANCED_FACE('',(#714,#392),#518,.T.);
#4638=ADVANCED_FACE('',(#715),#4531,.F.);
#4639=ADVANCED_FACE('',(#716),#4532,.F.);
#4640=ADVANCED_FACE('',(#717),#4533,.F.);
#4641=ADVANCED_FACE('',(#718),#4534,.F.);
#4642=ADVANCED_FACE('',(#719),#4535,.F.);
#4643=ADVANCED_FACE('',(#720,#393),#519,.T.);
#4644=ADVANCED_FACE('',(#721,#394,#395,#396,#397,#398),#520,.T.);
#4645=ADVANCED_FACE('',(#722),#521,.T.);
#4646=ADVANCED_FACE('',(#723,#399,#400,#401,#402,#403),#522,.T.);
#4647=ADVANCED_FACE('',(#724),#523,.T.);
#4648=ADVANCED_FACE('',(#725,#404),#524,.T.);
#4649=ADVANCED_FACE('',(#726,#405,#406),#525,.F.);
#4650=ADVANCED_FACE('',(#727),#4536,.F.);
#4651=ADVANCED_FACE('',(#728,#407),#526,.T.);
#4652=ADVANCED_FACE('',(#729,#408),#527,.F.);
#4653=ADVANCED_FACE('',(#730),#4537,.F.);
#4654=ADVANCED_FACE('',(#731),#4538,.F.);
#4655=ADVANCED_FACE('',(#732,#409),#528,.F.);
#4656=ADVANCED_FACE('',(#733,#410),#529,.T.);
#4657=ADVANCED_FACE('',(#734),#4539,.F.);
#4658=ADVANCED_FACE('',(#735),#4540,.F.);
#4659=ADVANCED_FACE('',(#736,#411),#530,.T.);
#4660=ADVANCED_FACE('',(#737),#531,.F.);
#4661=ADVANCED_FACE('',(#738),#532,.T.);
#4662=ADVANCED_FACE('',(#739,#412),#533,.T.);
#4663=ADVANCED_FACE('',(#740),#534,.T.);
#4664=ADVANCED_FACE('',(#741),#535,.T.);
#4665=ADVANCED_FACE('',(#742,#413),#536,.T.);
#4666=ADVANCED_FACE('',(#743),#537,.F.);
#4667=ADVANCED_FACE('',(#744),#538,.T.);
#4668=ADVANCED_FACE('',(#745,#414),#539,.F.);
#4669=ADVANCED_FACE('',(#746),#540,.T.);
#4670=ADVANCED_FACE('',(#747),#541,.T.);
#4671=ADVANCED_FACE('',(#748),#542,.T.);
#4672=ADVANCED_FACE('',(#749),#543,.T.);
#4673=ADVANCED_FACE('',(#750),#544,.T.);
#4674=ADVANCED_FACE('',(#751),#545,.T.);
#4675=ADVANCED_FACE('',(#752),#546,.T.);
#4676=ADVANCED_FACE('',(#753),#4541,.F.);
#4677=ADVANCED_FACE('',(#754),#4542,.T.);
#4678=ADVANCED_FACE('',(#755,#415),#547,.F.);
#4679=ADVANCED_FACE('',(#756),#263,.T.);
#4680=ADVANCED_FACE('',(#757),#264,.T.);
#4681=ADVANCED_FACE('',(#758),#4543,.T.);
#4682=ADVANCED_FACE('',(#759,#416),#548,.T.);
#4683=ADVANCED_FACE('',(#760),#4544,.T.);
#4684=ADVANCED_FACE('',(#761),#549,.T.);
#4685=ADVANCED_FACE('',(#762),#4545,.F.);
#4686=ADVANCED_FACE('',(#763),#550,.F.);
#4687=ADVANCED_FACE('',(#764),#4546,.F.);
#4688=ADVANCED_FACE('',(#765),#551,.F.);
#4689=ADVANCED_FACE('',(#766),#552,.F.);
#4690=ADVANCED_FACE('',(#767),#553,.F.);
#4691=ADVANCED_FACE('',(#768),#554,.F.);
#4692=ADVANCED_FACE('',(#769),#4547,.F.);
#4693=ADVANCED_FACE('',(#770),#4548,.F.);
#4694=ADVANCED_FACE('',(#771),#4549,.F.);
#4695=ADVANCED_FACE('',(#772),#555,.T.);
#4696=ADVANCED_FACE('',(#773),#556,.T.);
#4697=ADVANCED_FACE('',(#774),#557,.T.);
#4698=ADVANCED_FACE('',(#775),#558,.T.);
#4699=ADVANCED_FACE('',(#776),#4550,.F.);
#4700=ADVANCED_FACE('',(#777),#4551,.F.);
#4701=ADVANCED_FACE('',(#778),#4552,.F.);
#4702=ADVANCED_FACE('',(#779),#559,.F.);
#4703=ADVANCED_FACE('',(#780),#4553,.F.);
#4704=ADVANCED_FACE('',(#781,#417),#560,.T.);
#4705=ADVANCED_FACE('',(#782),#4554,.F.);
#4706=ADVANCED_FACE('',(#783),#4555,.F.);
#4707=ADVANCED_FACE('',(#784),#4556,.F.);
#4708=ADVANCED_FACE('',(#785),#4557,.F.);
#4709=ADVANCED_FACE('',(#786),#4558,.F.);
#4710=ADVANCED_FACE('',(#787,#418,#419,#420,#421),#561,.T.);
#4711=ADVANCED_FACE('',(#788),#562,.T.);
#4712=ADVANCED_FACE('',(#789,#422,#423,#424,#425,#426),#563,.T.);
#4713=ADVANCED_FACE('',(#790),#564,.T.);
#4714=ADVANCED_FACE('',(#791,#427),#565,.T.);
#4715=ADVANCED_FACE('',(#792,#428,#429),#566,.F.);
#4716=ADVANCED_FACE('',(#793),#4559,.F.);
#4717=ADVANCED_FACE('',(#794,#430),#567,.T.);
#4718=ADVANCED_FACE('',(#795,#431),#568,.F.);
#4719=ADVANCED_FACE('',(#796),#4560,.F.);
#4720=ADVANCED_FACE('',(#797),#4561,.F.);
#4721=ADVANCED_FACE('',(#798,#432),#569,.F.);
#4722=ADVANCED_FACE('',(#799,#433),#570,.T.);
#4723=ADVANCED_FACE('',(#800),#4562,.F.);
#4724=ADVANCED_FACE('',(#801),#4563,.F.);
#4725=ADVANCED_FACE('',(#802,#434),#571,.T.);
#4726=ADVANCED_FACE('',(#803),#572,.F.);
#4727=ADVANCED_FACE('',(#804),#573,.T.);
#4728=ADVANCED_FACE('',(#805,#435),#574,.T.);
#4729=ADVANCED_FACE('',(#806),#575,.T.);
#4730=ADVANCED_FACE('',(#807),#576,.T.);
#4731=ADVANCED_FACE('',(#808,#436),#577,.T.);
#4732=ADVANCED_FACE('',(#809),#578,.F.);
#4733=ADVANCED_FACE('',(#810),#579,.T.);
#4734=ADVANCED_FACE('',(#811,#437),#580,.F.);
#4735=ADVANCED_FACE('',(#812),#581,.T.);
#4736=ADVANCED_FACE('',(#813),#582,.T.);
#4737=ADVANCED_FACE('',(#814),#583,.T.);
#4738=ADVANCED_FACE('',(#815),#584,.T.);
#4739=ADVANCED_FACE('',(#816),#585,.T.);
#4740=ADVANCED_FACE('',(#817),#586,.T.);
#4741=ADVANCED_FACE('',(#818),#587,.T.);
#4742=ADVANCED_FACE('',(#819),#4564,.F.);
#4743=ADVANCED_FACE('',(#820),#4565,.T.);
#4744=ADVANCED_FACE('',(#821,#438),#588,.F.);
#4745=ADVANCED_FACE('',(#822),#265,.T.);
#4746=ADVANCED_FACE('',(#823),#266,.T.);
#4747=ADVANCED_FACE('',(#824),#4566,.T.);
#4748=ADVANCED_FACE('',(#825,#439),#589,.T.);
#4749=ADVANCED_FACE('',(#826),#4567,.T.);
#4750=ADVANCED_FACE('',(#827),#590,.T.);
#4751=ADVANCED_FACE('',(#828),#4568,.F.);
#4752=ADVANCED_FACE('',(#829),#4569,.T.);
#4753=ADVANCED_FACE('',(#830,#440),#591,.T.);
#4754=ADVANCED_FACE('',(#831,#441),#592,.F.);
#4755=ADVANCED_FACE('',(#832),#4570,.F.);
#4756=ADVANCED_FACE('',(#833),#4571,.T.);
#4757=ADVANCED_FACE('',(#834,#442),#593,.T.);
#4758=ADVANCED_FACE('',(#835,#443),#594,.F.);
#4759=ADVANCED_FACE('',(#836),#4572,.F.);
#4760=ADVANCED_FACE('',(#837),#4573,.T.);
#4761=ADVANCED_FACE('',(#838,#444),#595,.T.);
#4762=ADVANCED_FACE('',(#839,#445),#596,.F.);
#4763=ADVANCED_FACE('',(#840),#4574,.F.);
#4764=ADVANCED_FACE('',(#841),#4575,.F.);
#4765=ADVANCED_FACE('',(#842),#4576,.F.);
#4766=ADVANCED_FACE('',(#843,#446),#597,.F.);
#4767=ADVANCED_FACE('',(#844),#4577,.F.);
#4768=ADVANCED_FACE('',(#845,#447),#598,.F.);
#4769=ADVANCED_FACE('',(#846),#4578,.F.);
#4770=ADVANCED_FACE('',(#847),#4579,.F.);
#4771=ADVANCED_FACE('',(#848),#599,.T.);
#4772=ADVANCED_FACE('',(#849),#600,.T.);
#4773=ADVANCED_FACE('',(#850),#601,.T.);
#4774=ADVANCED_FACE('',(#851),#602,.T.);
#4775=ADVANCED_FACE('',(#852,#448,#449,#450,#451),#603,.T.);
#4776=ADVANCED_FACE('',(#853,#452,#453,#454,#455),#604,.F.);
#4777=ADVANCED_FACE('',(#854),#605,.T.);
#4778=ADVANCED_FACE('',(#855),#267,.T.);
#4779=ADVANCED_FACE('',(#856),#4580,.T.);
#4780=ADVANCED_FACE('',(#857),#268,.T.);
#4781=ADVANCED_FACE('',(#858,#456),#606,.T.);
#4782=ADVANCED_FACE('',(#859),#269,.T.);
#4783=ADVANCED_FACE('',(#860),#4581,.T.);
#4784=ADVANCED_FACE('',(#861),#270,.T.);
#4785=ADVANCED_FACE('',(#862),#607,.T.);
#4786=ADVANCED_FACE('',(#863),#608,.F.);
#4787=ADVANCED_FACE('',(#864),#609,.F.);
#4788=ADVANCED_FACE('',(#865),#610,.F.);
#4789=ADVANCED_FACE('',(#866),#611,.F.);
#4790=ADVANCED_FACE('',(#867),#612,.F.);
#4791=ADVANCED_FACE('',(#868),#613,.F.);
#4792=ADVANCED_FACE('',(#869),#614,.F.);
#4793=ADVANCED_FACE('',(#870),#615,.F.);
#4794=ADVANCED_FACE('',(#871),#4582,.F.);
#4795=ADVANCED_FACE('',(#872,#457),#616,.T.);
#4796=ADVANCED_FACE('',(#873,#458),#617,.T.);
#4797=ADVANCED_FACE('',(#874,#459),#618,.F.);
#4798=ADVANCED_FACE('',(#875),#619,.T.);
#4799=ADVANCED_FACE('',(#876),#620,.T.);
#4800=ADVANCED_FACE('',(#877),#621,.T.);
#4801=ADVANCED_FACE('',(#878),#622,.T.);
#4802=ADVANCED_FACE('',(#879),#623,.T.);
#4803=ADVANCED_FACE('',(#880),#624,.T.);
#4804=ADVANCED_FACE('',(#881,#460),#625,.T.);
#4805=ADVANCED_FACE('',(#882),#4583,.F.);
#4806=ADVANCED_FACE('',(#883,#461),#626,.T.);
#4807=ADVANCED_FACE('',(#884),#4584,.T.);
#4808=ADVANCED_FACE('',(#885),#4585,.T.);
#4809=ADVANCED_FACE('',(#886,#462),#627,.T.);
#4810=ADVANCED_FACE('',(#887),#4586,.F.);
#4811=ADVANCED_FACE('',(#888,#463),#628,.T.);
#4812=ADVANCED_FACE('',(#889),#4587,.T.);
#4813=ADVANCED_FACE('',(#890,#464),#629,.T.);
#4814=ADVANCED_FACE('',(#891),#4588,.T.);
#4815=ADVANCED_FACE('',(#892,#465),#630,.T.);
#4816=ADVANCED_FACE('',(#893),#4589,.F.);
#4817=ADVANCED_FACE('',(#894),#31,.T.);
#4818=ADVANCED_FACE('',(#895),#4590,.F.);
#4819=ADVANCED_FACE('',(#896,#466),#631,.F.);
#4820=ADVANCED_FACE('',(#897,#467),#632,.T.);
#4821=ADVANCED_FACE('',(#898),#4591,.F.);
#4822=ADVANCED_FACE('',(#899),#4592,.F.);
#4823=ADVANCED_FACE('',(#900),#4593,.T.);
#4824=ADVANCED_FACE('',(#901,#468),#633,.T.);
#4825=ADVANCED_FACE('',(#902,#469),#634,.F.);
#4826=ADVANCED_FACE('',(#903),#32,.T.);
#4827=ADVANCED_FACE('',(#904),#4594,.T.);
#4828=ADVANCED_FACE('',(#905),#635,.T.);
#4829=ADVANCED_FACE('',(#906),#636,.F.);
#4830=ADVANCED_FACE('',(#907),#271,.F.);
#4831=ADVANCED_FACE('',(#908),#4595,.F.);
#4832=ADVANCED_FACE('',(#909,#470),#637,.T.);
#4833=ADVANCED_FACE('',(#910),#4596,.T.);
#4834=ADVANCED_FACE('',(#911,#471),#638,.F.);
#4835=ADVANCED_FACE('',(#912),#272,.T.);
#4836=ADVANCED_FACE('',(#913),#273,.T.);
#4837=ADVANCED_FACE('',(#914),#639,.T.);
#4838=ADVANCED_FACE('',(#915),#640,.T.);
#4839=ADVANCED_FACE('',(#916),#641,.T.);
#4840=ADVANCED_FACE('',(#917),#4597,.F.);
#4841=ADVANCED_FACE('',(#918),#642,.T.);
#4842=ADVANCED_FACE('',(#919),#643,.T.);
#4843=ADVANCED_FACE('',(#920),#644,.T.);
#4844=ADVANCED_FACE('',(#921,#472),#645,.T.);
#4845=ADVANCED_FACE('',(#922,#473),#646,.F.);
#4846=ADVANCED_FACE('',(#923),#4598,.F.);
#4847=ADVANCED_FACE('',(#924,#474),#647,.T.);
#4848=ADVANCED_FACE('',(#925),#4599,.T.);
#4849=ADVANCED_FACE('',(#926,#475),#648,.F.);
#4850=ADVANCED_FACE('',(#927,#476),#649,.T.);
#4851=ADVANCED_FACE('',(#928),#4600,.T.);
#4852=ADVANCED_FACE('',(#929),#4601,.F.);
#4853=ADVANCED_FACE('',(#930),#4602,.T.);
#4854=ADVANCED_FACE('',(#931,#477),#650,.T.);
#4855=ADVANCED_FACE('',(#932,#478),#651,.F.);
#4856=ADVANCED_FACE('',(#933),#33,.T.);
#4857=ADVANCED_FACE('',(#934),#4603,.F.);
#4858=ADVANCED_FACE('',(#935),#652,.T.);
#4859=ADVANCED_FACE('',(#936),#4604,.T.);
#4860=ADVANCED_FACE('',(#937,#479),#653,.T.);
#4861=ADVANCED_FACE('',(#938),#654,.F.);
#4862=ADVANCED_FACE('',(#939),#655,.T.);
#4863=ADVANCED_FACE('',(#940),#274,.T.);
#4864=ADVANCED_FACE('',(#941),#4605,.T.);
#4865=ADVANCED_FACE('',(#942),#275,.T.);
#4866=ADVANCED_FACE('',(#943,#480),#656,.T.);
#4867=ADVANCED_FACE('',(#944),#276,.T.);
#4868=ADVANCED_FACE('',(#945),#4606,.T.);
#4869=ADVANCED_FACE('',(#946),#277,.T.);
#4870=ADVANCED_FACE('',(#947),#657,.T.);
#4871=ADVANCED_FACE('',(#948),#658,.F.);
#4872=ADVANCED_FACE('',(#949),#659,.F.);
#4873=ADVANCED_FACE('',(#950),#660,.F.);
#4874=ADVANCED_FACE('',(#951),#661,.F.);
#4875=ADVANCED_FACE('',(#952),#662,.F.);
#4876=ADVANCED_FACE('',(#953),#663,.F.);
#4877=ADVANCED_FACE('',(#954),#664,.F.);
#4878=ADVANCED_FACE('',(#955),#665,.F.);
#4879=ADVANCED_FACE('',(#956),#4607,.F.);
#4880=ADVANCED_FACE('',(#957),#4608,.F.);
#4881=ADVANCED_FACE('',(#958),#666,.T.);
#4882=ADVANCED_FACE('',(#959),#4609,.F.);
#4883=ADVANCED_FACE('',(#960),#667,.T.);
#4884=ADVANCED_FACE('',(#961,#481),#4610,.F.);
#4885=ADVANCED_FACE('',(#962,#482),#668,.F.);
#4886=ADVANCED_FACE('',(#963,#483),#669,.F.);
#4887=ADVANCED_FACE('',(#964,#484),#670,.F.);
#4888=ADVANCED_FACE('',(#965),#671,.F.);
#4889=ADVANCED_FACE('',(#966),#672,.T.);
#4890=ADVANCED_FACE('',(#967),#673,.T.);
#4891=ADVANCED_FACE('',(#968,#485),#674,.T.);
#4892=ADVANCED_FACE('',(#969,#486),#675,.T.);
#4893=ADVANCED_FACE('',(#970,#487),#676,.T.);
#4894=ADVANCED_FACE('',(#971,#488),#677,.T.);
#4895=ADVANCED_FACE('',(#972),#678,.F.);
#4896=ADVANCED_FACE('',(#973),#679,.F.);
#4897=ADVANCED_FACE('',(#974),#680,.F.);
#4898=ADVANCED_FACE('',(#975),#681,.F.);
#4899=ADVANCED_FACE('',(#976),#682,.F.);
#4900=ADVANCED_FACE('',(#977),#683,.F.);
#4901=ADVANCED_FACE('',(#978),#684,.F.);
#4902=ADVANCED_FACE('',(#979,#489),#685,.T.);
#4903=ADVANCED_FACE('',(#980),#278,.T.);
#4904=ADVANCED_FACE('',(#981),#4611,.T.);
#4905=ADVANCED_FACE('',(#982),#279,.T.);
#4906=ADVANCED_FACE('',(#983),#686,.T.);
#4907=ADVANCED_FACE('',(#984),#4612,.F.);
#4908=ADVANCED_FACE('',(#985),#687,.T.);
#4909=ADVANCED_FACE('',(#986),#280,.T.);
#4910=ADVANCED_FACE('',(#987),#4613,.T.);
#4911=ADVANCED_FACE('',(#988,#490),#688,.T.);
#4912=ADVANCED_FACE('',(#989,#491),#4614,.T.);
#4913=ADVANCED_FACE('',(#990),#281,.T.);
#4914=ADVANCED_FACE('',(#991),#689,.T.);
#4915=ADVANCED_FACE('',(#992),#4615,.F.);
#4916=ADVANCED_FACE('',(#993),#4616,.T.);
#4917=ADVANCED_FACE('',(#994,#492),#690,.T.);
#4918=ADVANCED_FACE('',(#995,#493),#691,.F.);
#4919=ADVANCED_FACE('',(#996,#494),#34,.T.);
#4920=ADVANCED_FACE('',(#997),#692,.F.);
#4921=ADVANCED_FACE('',(#998),#693,.T.);
#4922=ADVANCED_FACE('',(#999),#4617,.T.);
#4923=ADVANCED_FACE('',(#1000),#694,.F.);
#4924=CLOSED_SHELL('',(#4618,#4619,#4620,#4621,#4622,#4623,#4624,#4625,
#4626,#4627,#4628,#4629,#4630,#4631,#4632,#4633,#4634,#4635,#4636,#4637,
#4638,#4639,#4640,#4641,#4642,#4643,#4644,#4645,#4646,#4647,#4648,#4649));
#4925=CLOSED_SHELL('',(#4650,#4651,#4652,#4653,#4654,#4655,#4656,#4657,
#4658,#4659,#4660,#4661,#4662,#4663,#4664,#4665,#4666,#4667,#4668,#4669,
#4670,#4671,#4672,#4673,#4674,#4675,#4676,#4677,#4678));
#4926=CLOSED_SHELL('',(#4679,#4680,#4681,#4682,#4683,#4684));
#4927=CLOSED_SHELL('',(#4685,#4686,#4687,#4688,#4689,#4690,#4691,#4692,
#4693,#4694,#4695,#4696,#4697,#4698,#4699,#4700,#4701,#4702,#4703,#4704,
#4705,#4706,#4707,#4708,#4709,#4710,#4711,#4712,#4713,#4714,#4715));
#4928=CLOSED_SHELL('',(#4716,#4717,#4718,#4719,#4720,#4721,#4722,#4723,
#4724,#4725,#4726,#4727,#4728,#4729,#4730,#4731,#4732,#4733,#4734,#4735,
#4736,#4737,#4738,#4739,#4740,#4741,#4742,#4743,#4744));
#4929=CLOSED_SHELL('',(#4745,#4746,#4747,#4748,#4749,#4750));
#4930=CLOSED_SHELL('',(#4751,#4752,#4753,#4754));
#4931=CLOSED_SHELL('',(#4755,#4756,#4757,#4758));
#4932=CLOSED_SHELL('',(#4759,#4760,#4761,#4762));
#4933=CLOSED_SHELL('',(#4763,#4764,#4765,#4766,#4767,#4768,#4769,#4770,
#4771,#4772,#4773,#4774,#4775,#4776));
#4934=CLOSED_SHELL('',(#4777,#4778,#4779,#4780,#4781,#4782,#4783,#4784,
#4785));
#4935=CLOSED_SHELL('',(#4786,#4787,#4788,#4789,#4790,#4791,#4792,#4793));
#4936=CLOSED_SHELL('',(#4794,#4795,#4796,#4797,#4798,#4799,#4800,#4801,
#4802,#4803,#4804,#4805,#4806,#4807,#4808,#4809,#4810));
#4937=CLOSED_SHELL('',(#4811,#4812,#4813,#4814,#4815,#4816));
#4938=CLOSED_SHELL('',(#4817));
#4939=CLOSED_SHELL('',(#4818,#4819,#4820,#4821,#4822,#4823,#4824,#4825));
#4940=CLOSED_SHELL('',(#4826));
#4941=CLOSED_SHELL('',(#4827,#4828,#4829));
#4942=CLOSED_SHELL('',(#4830,#4831,#4832,#4833,#4834));
#4943=CLOSED_SHELL('',(#4835,#4836,#4837,#4838,#4839,#4840,#4841,#4842,
#4843,#4844,#4845));
#4944=CLOSED_SHELL('',(#4846,#4847,#4848,#4849,#4850,#4851,#4852,#4853,
#4854,#4855));
#4945=CLOSED_SHELL('',(#4856));
#4946=CLOSED_SHELL('',(#4857,#4858,#4859,#4860,#4861));
#4947=CLOSED_SHELL('',(#4862,#4863,#4864,#4865,#4866,#4867,#4868,#4869,
#4870));
#4948=CLOSED_SHELL('',(#4871,#4872,#4873,#4874,#4875,#4876,#4877,#4878));
#4949=CLOSED_SHELL('',(#4879,#4880,#4881,#4882,#4883,#4884,#4885,#4886,
#4887,#4888,#4889,#4890,#4891,#4892,#4893,#4894));
#4950=CLOSED_SHELL('',(#4895,#4896,#4897,#4898,#4899,#4900,#4901,#4902,
#4903,#4904,#4905,#4906));
#4951=CLOSED_SHELL('',(#4907,#4908,#4909,#4910,#4911,#4912,#4913,#4914));
#4952=CLOSED_SHELL('',(#4915,#4916,#4917,#4918));
#4953=CLOSED_SHELL('',(#4919,#4920,#4921,#4922,#4923));
#4954=DERIVED_UNIT_ELEMENT(#5010,1.);
#4955=DERIVED_UNIT_ELEMENT(#9104,-3.);
#4956=DERIVED_UNIT_ELEMENT(#5010,1.);
#4957=DERIVED_UNIT_ELEMENT(#9104,-3.);
#4958=DERIVED_UNIT_ELEMENT(#5010,1.);
#4959=DERIVED_UNIT_ELEMENT(#9104,-3.);
#4960=DERIVED_UNIT_ELEMENT(#5010,1.);
#4961=DERIVED_UNIT_ELEMENT(#9104,-3.);
#4962=DERIVED_UNIT_ELEMENT(#5010,1.);
#4963=DERIVED_UNIT_ELEMENT(#9104,-3.);
#4964=DERIVED_UNIT_ELEMENT(#5010,1.);
#4965=DERIVED_UNIT_ELEMENT(#9104,-3.);
#4966=DERIVED_UNIT_ELEMENT(#5010,1.);
#4967=DERIVED_UNIT_ELEMENT(#9104,-3.);
#4968=DERIVED_UNIT_ELEMENT(#5010,1.);
#4969=DERIVED_UNIT_ELEMENT(#9104,-3.);
#4970=DERIVED_UNIT_ELEMENT(#5010,1.);
#4971=DERIVED_UNIT_ELEMENT(#9104,-3.);
#4972=DERIVED_UNIT_ELEMENT(#5010,1.);
#4973=DERIVED_UNIT_ELEMENT(#9104,-3.);
#4974=DERIVED_UNIT_ELEMENT(#5010,1.);
#4975=DERIVED_UNIT_ELEMENT(#9104,-3.);
#4976=DERIVED_UNIT_ELEMENT(#5010,1.);
#4977=DERIVED_UNIT_ELEMENT(#9104,-3.);
#4978=DERIVED_UNIT_ELEMENT(#5010,1.);
#4979=DERIVED_UNIT_ELEMENT(#9104,-3.);
#4980=DERIVED_UNIT_ELEMENT(#5010,1.);
#4981=DERIVED_UNIT_ELEMENT(#9104,-3.);
#4982=DERIVED_UNIT_ELEMENT(#5010,1.);
#4983=DERIVED_UNIT_ELEMENT(#9104,-3.);
#4984=DERIVED_UNIT_ELEMENT(#5010,1.);
#4985=DERIVED_UNIT_ELEMENT(#9104,-3.);
#4986=DERIVED_UNIT_ELEMENT(#5010,1.);
#4987=DERIVED_UNIT_ELEMENT(#9104,-3.);
#4988=DERIVED_UNIT_ELEMENT(#5010,1.);
#4989=DERIVED_UNIT_ELEMENT(#9104,-3.);
#4990=DERIVED_UNIT_ELEMENT(#5010,1.);
#4991=DERIVED_UNIT_ELEMENT(#9104,-3.);
#4992=DERIVED_UNIT_ELEMENT(#5010,1.);
#4993=DERIVED_UNIT_ELEMENT(#9104,-3.);
#4994=DERIVED_UNIT_ELEMENT(#5010,1.);
#4995=DERIVED_UNIT_ELEMENT(#9104,-3.);
#4996=DERIVED_UNIT_ELEMENT(#5010,1.);
#4997=DERIVED_UNIT_ELEMENT(#9104,-3.);
#4998=DERIVED_UNIT_ELEMENT(#5010,1.);
#4999=DERIVED_UNIT_ELEMENT(#9104,-3.);
#5000=DERIVED_UNIT_ELEMENT(#5010,1.);
#5001=DERIVED_UNIT_ELEMENT(#9104,-3.);
#5002=DERIVED_UNIT_ELEMENT(#5010,1.);
#5003=DERIVED_UNIT_ELEMENT(#9104,-3.);
#5004=DERIVED_UNIT_ELEMENT(#5010,1.);
#5005=DERIVED_UNIT_ELEMENT(#9104,-3.);
#5006=DERIVED_UNIT_ELEMENT(#5010,1.);
#5007=DERIVED_UNIT_ELEMENT(#9104,-3.);
#5008=DERIVED_UNIT_ELEMENT(#5010,1.);
#5009=DERIVED_UNIT_ELEMENT(#9104,-3.);
#5010=(
MASS_UNIT()
NAMED_UNIT(*)
SI_UNIT(.KILO.,.GRAM.)
);
#5011=DERIVED_UNIT((#4954,#4955));
#5012=DERIVED_UNIT((#4956,#4957));
#5013=DERIVED_UNIT((#4958,#4959));
#5014=DERIVED_UNIT((#4960,#4961));
#5015=DERIVED_UNIT((#4962,#4963));
#5016=DERIVED_UNIT((#4964,#4965));
#5017=DERIVED_UNIT((#4966,#4967));
#5018=DERIVED_UNIT((#4968,#4969));
#5019=DERIVED_UNIT((#4970,#4971));
#5020=DERIVED_UNIT((#4972,#4973));
#5021=DERIVED_UNIT((#4974,#4975));
#5022=DERIVED_UNIT((#4976,#4977));
#5023=DERIVED_UNIT((#4978,#4979));
#5024=DERIVED_UNIT((#4980,#4981));
#5025=DERIVED_UNIT((#4982,#4983));
#5026=DERIVED_UNIT((#4984,#4985));
#5027=DERIVED_UNIT((#4986,#4987));
#5028=DERIVED_UNIT((#4988,#4989));
#5029=DERIVED_UNIT((#4990,#4991));
#5030=DERIVED_UNIT((#4992,#4993));
#5031=DERIVED_UNIT((#4994,#4995));
#5032=DERIVED_UNIT((#4996,#4997));
#5033=DERIVED_UNIT((#4998,#4999));
#5034=DERIVED_UNIT((#5000,#5001));
#5035=DERIVED_UNIT((#5002,#5003));
#5036=DERIVED_UNIT((#5004,#5005));
#5037=DERIVED_UNIT((#5006,#5007));
#5038=DERIVED_UNIT((#5008,#5009));
#5039=MEASURE_REPRESENTATION_ITEM('density measure',
POSITIVE_RATIO_MEASURE(7850.),#5011);
#5040=MEASURE_REPRESENTATION_ITEM('density measure',
POSITIVE_RATIO_MEASURE(7850.),#5012);
#5041=MEASURE_REPRESENTATION_ITEM('density measure',
POSITIVE_RATIO_MEASURE(7850.),#5013);
#5042=MEASURE_REPRESENTATION_ITEM('density measure',
POSITIVE_RATIO_MEASURE(7850.),#5014);
#5043=MEASURE_REPRESENTATION_ITEM('density measure',
POSITIVE_RATIO_MEASURE(7850.),#5015);
#5044=MEASURE_REPRESENTATION_ITEM('density measure',
POSITIVE_RATIO_MEASURE(7850.),#5016);
#5045=MEASURE_REPRESENTATION_ITEM('density measure',
POSITIVE_RATIO_MEASURE(7850.),#5017);
#5046=MEASURE_REPRESENTATION_ITEM('density measure',
POSITIVE_RATIO_MEASURE(7850.),#5018);
#5047=MEASURE_REPRESENTATION_ITEM('density measure',
POSITIVE_RATIO_MEASURE(7850.),#5019);
#5048=MEASURE_REPRESENTATION_ITEM('density measure',
POSITIVE_RATIO_MEASURE(7850.),#5020);
#5049=MEASURE_REPRESENTATION_ITEM('density measure',
POSITIVE_RATIO_MEASURE(7850.),#5021);
#5050=MEASURE_REPRESENTATION_ITEM('density measure',
POSITIVE_RATIO_MEASURE(7850.),#5022);
#5051=MEASURE_REPRESENTATION_ITEM('density measure',
POSITIVE_RATIO_MEASURE(7850.),#5023);
#5052=MEASURE_REPRESENTATION_ITEM('density measure',
POSITIVE_RATIO_MEASURE(7850.),#5024);
#5053=MEASURE_REPRESENTATION_ITEM('density measure',
POSITIVE_RATIO_MEASURE(7850.),#5025);
#5054=MEASURE_REPRESENTATION_ITEM('density measure',
POSITIVE_RATIO_MEASURE(7850.),#5026);
#5055=MEASURE_REPRESENTATION_ITEM('density measure',
POSITIVE_RATIO_MEASURE(7850.),#5027);
#5056=MEASURE_REPRESENTATION_ITEM('density measure',
POSITIVE_RATIO_MEASURE(7850.),#5028);
#5057=MEASURE_REPRESENTATION_ITEM('density measure',
POSITIVE_RATIO_MEASURE(7850.),#5029);
#5058=MEASURE_REPRESENTATION_ITEM('density measure',
POSITIVE_RATIO_MEASURE(7850.),#5030);
#5059=MEASURE_REPRESENTATION_ITEM('density measure',
POSITIVE_RATIO_MEASURE(7850.),#5031);
#5060=MEASURE_REPRESENTATION_ITEM('density measure',
POSITIVE_RATIO_MEASURE(7850.),#5032);
#5061=MEASURE_REPRESENTATION_ITEM('density measure',
POSITIVE_RATIO_MEASURE(7850.),#5033);
#5062=MEASURE_REPRESENTATION_ITEM('density measure',
POSITIVE_RATIO_MEASURE(7850.),#5034);
#5063=MEASURE_REPRESENTATION_ITEM('density measure',
POSITIVE_RATIO_MEASURE(7850.),#5035);
#5064=MEASURE_REPRESENTATION_ITEM('density measure',
POSITIVE_RATIO_MEASURE(7850.),#5036);
#5065=MEASURE_REPRESENTATION_ITEM('density measure',
POSITIVE_RATIO_MEASURE(7850.),#5037);
#5066=MEASURE_REPRESENTATION_ITEM('density measure',
POSITIVE_RATIO_MEASURE(7850.),#5038);
#5067=PROPERTY_DEFINITION_REPRESENTATION(#5207,#5123);
#5068=PROPERTY_DEFINITION_REPRESENTATION(#5208,#5124);
#5069=PROPERTY_DEFINITION_REPRESENTATION(#5209,#5125);
#5070=PROPERTY_DEFINITION_REPRESENTATION(#5210,#5126);
#5071=PROPERTY_DEFINITION_REPRESENTATION(#5211,#5127);
#5072=PROPERTY_DEFINITION_REPRESENTATION(#5212,#5128);
#5073=PROPERTY_DEFINITION_REPRESENTATION(#5213,#5129);
#5074=PROPERTY_DEFINITION_REPRESENTATION(#5214,#5130);
#5075=PROPERTY_DEFINITION_REPRESENTATION(#5215,#5131);
#5076=PROPERTY_DEFINITION_REPRESENTATION(#5216,#5132);
#5077=PROPERTY_DEFINITION_REPRESENTATION(#5217,#5133);
#5078=PROPERTY_DEFINITION_REPRESENTATION(#5218,#5134);
#5079=PROPERTY_DEFINITION_REPRESENTATION(#5219,#5135);
#5080=PROPERTY_DEFINITION_REPRESENTATION(#5220,#5136);
#5081=PROPERTY_DEFINITION_REPRESENTATION(#5221,#5137);
#5082=PROPERTY_DEFINITION_REPRESENTATION(#5222,#5138);
#5083=PROPERTY_DEFINITION_REPRESENTATION(#5223,#5139);
#5084=PROPERTY_DEFINITION_REPRESENTATION(#5224,#5140);
#5085=PROPERTY_DEFINITION_REPRESENTATION(#5225,#5141);
#5086=PROPERTY_DEFINITION_REPRESENTATION(#5226,#5142);
#5087=PROPERTY_DEFINITION_REPRESENTATION(#5227,#5143);
#5088=PROPERTY_DEFINITION_REPRESENTATION(#5228,#5144);
#5089=PROPERTY_DEFINITION_REPRESENTATION(#5229,#5145);
#5090=PROPERTY_DEFINITION_REPRESENTATION(#5230,#5146);
#5091=PROPERTY_DEFINITION_REPRESENTATION(#5231,#5147);
#5092=PROPERTY_DEFINITION_REPRESENTATION(#5232,#5148);
#5093=PROPERTY_DEFINITION_REPRESENTATION(#5233,#5149);
#5094=PROPERTY_DEFINITION_REPRESENTATION(#5234,#5150);
#5095=PROPERTY_DEFINITION_REPRESENTATION(#5235,#5151);
#5096=PROPERTY_DEFINITION_REPRESENTATION(#5236,#5152);
#5097=PROPERTY_DEFINITION_REPRESENTATION(#5237,#5153);
#5098=PROPERTY_DEFINITION_REPRESENTATION(#5238,#5154);
#5099=PROPERTY_DEFINITION_REPRESENTATION(#5239,#5155);
#5100=PROPERTY_DEFINITION_REPRESENTATION(#5240,#5156);
#5101=PROPERTY_DEFINITION_REPRESENTATION(#5241,#5157);
#5102=PROPERTY_DEFINITION_REPRESENTATION(#5242,#5158);
#5103=PROPERTY_DEFINITION_REPRESENTATION(#5243,#5159);
#5104=PROPERTY_DEFINITION_REPRESENTATION(#5244,#5160);
#5105=PROPERTY_DEFINITION_REPRESENTATION(#5245,#5161);
#5106=PROPERTY_DEFINITION_REPRESENTATION(#5246,#5162);
#5107=PROPERTY_DEFINITION_REPRESENTATION(#5247,#5163);
#5108=PROPERTY_DEFINITION_REPRESENTATION(#5248,#5164);
#5109=PROPERTY_DEFINITION_REPRESENTATION(#5249,#5165);
#5110=PROPERTY_DEFINITION_REPRESENTATION(#5250,#5166);
#5111=PROPERTY_DEFINITION_REPRESENTATION(#5251,#5167);
#5112=PROPERTY_DEFINITION_REPRESENTATION(#5252,#5168);
#5113=PROPERTY_DEFINITION_REPRESENTATION(#5253,#5169);
#5114=PROPERTY_DEFINITION_REPRESENTATION(#5254,#5170);
#5115=PROPERTY_DEFINITION_REPRESENTATION(#5255,#5171);
#5116=PROPERTY_DEFINITION_REPRESENTATION(#5256,#5172);
#5117=PROPERTY_DEFINITION_REPRESENTATION(#5257,#5173);
#5118=PROPERTY_DEFINITION_REPRESENTATION(#5258,#5174);
#5119=PROPERTY_DEFINITION_REPRESENTATION(#5259,#5175);
#5120=PROPERTY_DEFINITION_REPRESENTATION(#5260,#5176);
#5121=PROPERTY_DEFINITION_REPRESENTATION(#5261,#5177);
#5122=PROPERTY_DEFINITION_REPRESENTATION(#5262,#5178);
#5123=REPRESENTATION('material name',(#5179),#9072);
#5124=REPRESENTATION('density',(#5039),#9072);
#5125=REPRESENTATION('material name',(#5180),#9073);
#5126=REPRESENTATION('density',(#5040),#9073);
#5127=REPRESENTATION('material name',(#5181),#9074);
#5128=REPRESENTATION('density',(#5041),#9074);
#5129=REPRESENTATION('material name',(#5182),#9075);
#5130=REPRESENTATION('density',(#5042),#9075);
#5131=REPRESENTATION('material name',(#5183),#9076);
#5132=REPRESENTATION('density',(#5043),#9076);
#5133=REPRESENTATION('material name',(#5184),#9077);
#5134=REPRESENTATION('density',(#5044),#9077);
#5135=REPRESENTATION('material name',(#5185),#9078);
#5136=REPRESENTATION('density',(#5045),#9078);
#5137=REPRESENTATION('material name',(#5186),#9079);
#5138=REPRESENTATION('density',(#5046),#9079);
#5139=REPRESENTATION('material name',(#5187),#9080);
#5140=REPRESENTATION('density',(#5047),#9080);
#5141=REPRESENTATION('material name',(#5188),#9081);
#5142=REPRESENTATION('density',(#5048),#9081);
#5143=REPRESENTATION('material name',(#5189),#9082);
#5144=REPRESENTATION('density',(#5049),#9082);
#5145=REPRESENTATION('material name',(#5190),#9084);
#5146=REPRESENTATION('density',(#5050),#9084);
#5147=REPRESENTATION('material name',(#5191),#9085);
#5148=REPRESENTATION('density',(#5051),#9085);
#5149=REPRESENTATION('material name',(#5192),#9086);
#5150=REPRESENTATION('density',(#5052),#9086);
#5151=REPRESENTATION('material name',(#5193),#9087);
#5152=REPRESENTATION('density',(#5053),#9087);
#5153=REPRESENTATION('material name',(#5194),#9088);
#5154=REPRESENTATION('density',(#5054),#9088);
#5155=REPRESENTATION('material name',(#5195),#9089);
#5156=REPRESENTATION('density',(#5055),#9089);
#5157=REPRESENTATION('material name',(#5196),#9090);
#5158=REPRESENTATION('density',(#5056),#9090);
#5159=REPRESENTATION('material name',(#5197),#9091);
#5160=REPRESENTATION('density',(#5057),#9091);
#5161=REPRESENTATION('material name',(#5198),#9093);
#5162=REPRESENTATION('density',(#5058),#9093);
#5163=REPRESENTATION('material name',(#5199),#9094);
#5164=REPRESENTATION('density',(#5059),#9094);
#5165=REPRESENTATION('material name',(#5200),#9095);
#5166=REPRESENTATION('density',(#5060),#9095);
#5167=REPRESENTATION('material name',(#5201),#9096);
#5168=REPRESENTATION('density',(#5061),#9096);
#5169=REPRESENTATION('material name',(#5202),#9097);
#5170=REPRESENTATION('density',(#5062),#9097);
#5171=REPRESENTATION('material name',(#5203),#9098);
#5172=REPRESENTATION('density',(#5063),#9098);
#5173=REPRESENTATION('material name',(#5204),#9099);
#5174=REPRESENTATION('density',(#5064),#9099);
#5175=REPRESENTATION('material name',(#5205),#9100);
#5176=REPRESENTATION('density',(#5065),#9100);
#5177=REPRESENTATION('material name',(#5206),#9101);
#5178=REPRESENTATION('density',(#5066),#9101);
#5179=DESCRIPTIVE_REPRESENTATION_ITEM('Steel','Steel');
#5180=DESCRIPTIVE_REPRESENTATION_ITEM('Steel','Steel');
#5181=DESCRIPTIVE_REPRESENTATION_ITEM('Steel','Steel');
#5182=DESCRIPTIVE_REPRESENTATION_ITEM('Steel','Steel');
#5183=DESCRIPTIVE_REPRESENTATION_ITEM('Steel','Steel');
#5184=DESCRIPTIVE_REPRESENTATION_ITEM('Steel','Steel');
#5185=DESCRIPTIVE_REPRESENTATION_ITEM('Steel','Steel');
#5186=DESCRIPTIVE_REPRESENTATION_ITEM('Steel','Steel');
#5187=DESCRIPTIVE_REPRESENTATION_ITEM('Steel','Steel');
#5188=DESCRIPTIVE_REPRESENTATION_ITEM('Steel','Steel');
#5189=DESCRIPTIVE_REPRESENTATION_ITEM('Steel','Steel');
#5190=DESCRIPTIVE_REPRESENTATION_ITEM('Steel','Steel');
#5191=DESCRIPTIVE_REPRESENTATION_ITEM('Steel','Steel');
#5192=DESCRIPTIVE_REPRESENTATION_ITEM('Steel','Steel');
#5193=DESCRIPTIVE_REPRESENTATION_ITEM('Steel','Steel');
#5194=DESCRIPTIVE_REPRESENTATION_ITEM('Steel','Steel');
#5195=DESCRIPTIVE_REPRESENTATION_ITEM('Steel','Steel');
#5196=DESCRIPTIVE_REPRESENTATION_ITEM('Steel','Steel');
#5197=DESCRIPTIVE_REPRESENTATION_ITEM('Steel','Steel');
#5198=DESCRIPTIVE_REPRESENTATION_ITEM('Steel','Steel');
#5199=DESCRIPTIVE_REPRESENTATION_ITEM('Steel','Steel');
#5200=DESCRIPTIVE_REPRESENTATION_ITEM('Steel','Steel');
#5201=DESCRIPTIVE_REPRESENTATION_ITEM('Steel','Steel');
#5202=DESCRIPTIVE_REPRESENTATION_ITEM('Steel','Steel');
#5203=DESCRIPTIVE_REPRESENTATION_ITEM('Steel','Steel');
#5204=DESCRIPTIVE_REPRESENTATION_ITEM('Steel','Steel');
#5205=DESCRIPTIVE_REPRESENTATION_ITEM('Steel','Steel');
#5206=DESCRIPTIVE_REPRESENTATION_ITEM('Steel','Steel');
#5207=PROPERTY_DEFINITION('material property','material name',#9262);
#5208=PROPERTY_DEFINITION('material property','density of part',#9262);
#5209=PROPERTY_DEFINITION('material property','material name',#9263);
#5210=PROPERTY_DEFINITION('material property','density of part',#9263);
#5211=PROPERTY_DEFINITION('material property','material name',#9264);
#5212=PROPERTY_DEFINITION('material property','density of part',#9264);
#5213=PROPERTY_DEFINITION('material property','material name',#9265);
#5214=PROPERTY_DEFINITION('material property','density of part',#9265);
#5215=PROPERTY_DEFINITION('material property','material name',#9266);
#5216=PROPERTY_DEFINITION('material property','density of part',#9266);
#5217=PROPERTY_DEFINITION('material property','material name',#9267);
#5218=PROPERTY_DEFINITION('material property','density of part',#9267);
#5219=PROPERTY_DEFINITION('material property','material name',#9268);
#5220=PROPERTY_DEFINITION('material property','density of part',#9268);
#5221=PROPERTY_DEFINITION('material property','material name',#9269);
#5222=PROPERTY_DEFINITION('material property','density of part',#9269);
#5223=PROPERTY_DEFINITION('material property','material name',#9270);
#5224=PROPERTY_DEFINITION('material property','density of part',#9270);
#5225=PROPERTY_DEFINITION('material property','material name',#9271);
#5226=PROPERTY_DEFINITION('material property','density of part',#9271);
#5227=PROPERTY_DEFINITION('material property','material name',#9272);
#5228=PROPERTY_DEFINITION('material property','density of part',#9272);
#5229=PROPERTY_DEFINITION('material property','material name',#9274);
#5230=PROPERTY_DEFINITION('material property','density of part',#9274);
#5231=PROPERTY_DEFINITION('material property','material name',#9275);
#5232=PROPERTY_DEFINITION('material property','density of part',#9275);
#5233=PROPERTY_DEFINITION('material property','material name',#9276);
#5234=PROPERTY_DEFINITION('material property','density of part',#9276);
#5235=PROPERTY_DEFINITION('material property','material name',#9277);
#5236=PROPERTY_DEFINITION('material property','density of part',#9277);
#5237=PROPERTY_DEFINITION('material property','material name',#9278);
#5238=PROPERTY_DEFINITION('material property','density of part',#9278);
#5239=PROPERTY_DEFINITION('material property','material name',#9279);
#5240=PROPERTY_DEFINITION('material property','density of part',#9279);
#5241=PROPERTY_DEFINITION('material property','material name',#9280);
#5242=PROPERTY_DEFINITION('material property','density of part',#9280);
#5243=PROPERTY_DEFINITION('material property','material name',#9281);
#5244=PROPERTY_DEFINITION('material property','density of part',#9281);
#5245=PROPERTY_DEFINITION('material property','material name',#9283);
#5246=PROPERTY_DEFINITION('material property','density of part',#9283);
#5247=PROPERTY_DEFINITION('material property','material name',#9284);
#5248=PROPERTY_DEFINITION('material property','density of part',#9284);
#5249=PROPERTY_DEFINITION('material property','material name',#9285);
#5250=PROPERTY_DEFINITION('material property','density of part',#9285);
#5251=PROPERTY_DEFINITION('material property','material name',#9286);
#5252=PROPERTY_DEFINITION('material property','density of part',#9286);
#5253=PROPERTY_DEFINITION('material property','material name',#9287);
#5254=PROPERTY_DEFINITION('material property','density of part',#9287);
#5255=PROPERTY_DEFINITION('material property','material name',#9288);
#5256=PROPERTY_DEFINITION('material property','density of part',#9288);
#5257=PROPERTY_DEFINITION('material property','material name',#9289);
#5258=PROPERTY_DEFINITION('material property','density of part',#9289);
#5259=PROPERTY_DEFINITION('material property','material name',#9290);
#5260=PROPERTY_DEFINITION('material property','density of part',#9290);
#5261=PROPERTY_DEFINITION('material property','material name',#9291);
#5262=PROPERTY_DEFINITION('material property','density of part',#9291);
#5263=AXIS2_PLACEMENT_3D('',#7496,#5891,#5892);
#5264=AXIS2_PLACEMENT_3D('',#7497,#5893,#5894);
#5265=AXIS2_PLACEMENT_3D('',#7498,#5895,#5896);
#5266=AXIS2_PLACEMENT_3D('',#7499,#5897,#5898);
#5267=AXIS2_PLACEMENT_3D('',#7501,#5899,#5900);
#5268=AXIS2_PLACEMENT_3D('',#7504,#5902,#5903);
#5269=AXIS2_PLACEMENT_3D('',#7505,#5904,#5905);
#5270=AXIS2_PLACEMENT_3D('',#7506,#5906,#5907);
#5271=AXIS2_PLACEMENT_3D('',#7508,#5908,#5909);
#5272=AXIS2_PLACEMENT_3D('',#7511,#5911,#5912);
#5273=AXIS2_PLACEMENT_3D('',#7512,#5913,#5914);
#5274=AXIS2_PLACEMENT_3D('',#7513,#5915,#5916);
#5275=AXIS2_PLACEMENT_3D('',#7517,#5918,#5919);
#5276=AXIS2_PLACEMENT_3D('',#7518,#5920,#5921);
#5277=AXIS2_PLACEMENT_3D('',#7521,#5923,#5924);
#5278=AXIS2_PLACEMENT_3D('',#7522,#5925,#5926);
#5279=AXIS2_PLACEMENT_3D('',#7524,#5927,#5928);
#5280=AXIS2_PLACEMENT_3D('',#7525,#5929,#5930);
#5281=AXIS2_PLACEMENT_3D('',#7526,#5931,#5932);
#5282=AXIS2_PLACEMENT_3D('',#7531,#5935,#5936);
#5283=AXIS2_PLACEMENT_3D('',#7533,#5937,#5938);
#5284=AXIS2_PLACEMENT_3D('',#7537,#5940,#5941);
#5285=AXIS2_PLACEMENT_3D('',#7541,#5943,#5944);
#5286=AXIS2_PLACEMENT_3D('',#7544,#5946,#5947);
#5287=AXIS2_PLACEMENT_3D('',#7545,#5948,#5949);
#5288=AXIS2_PLACEMENT_3D('',#7546,#5950,#5951);
#5289=AXIS2_PLACEMENT_3D('',#7548,#5952,#5953);
#5290=AXIS2_PLACEMENT_3D('',#7549,#5954,#5955);
#5291=AXIS2_PLACEMENT_3D('',#7550,#5956,#5957);
#5292=AXIS2_PLACEMENT_3D('',#7551,#5958,#5959);
#5293=AXIS2_PLACEMENT_3D('',#7552,#5960,#5961);
#5294=AXIS2_PLACEMENT_3D('',#7553,#5962,#5963);
#5295=AXIS2_PLACEMENT_3D('',#7555,#5965,#5966);
#5296=AXIS2_PLACEMENT_3D('',#7556,#5967,#5968);
#5297=AXIS2_PLACEMENT_3D('',#7557,#5969,#5970);
#5298=AXIS2_PLACEMENT_3D('',#7558,#5971,#5972);
#5299=AXIS2_PLACEMENT_3D('',#7559,#5973,#5974);
#5300=AXIS2_PLACEMENT_3D('',#7560,#5975,#5976);
#5301=AXIS2_PLACEMENT_3D('',#7563,#5978,#5979);
#5302=AXIS2_PLACEMENT_3D('',#7564,#5980,#5981);
#5303=AXIS2_PLACEMENT_3D('',#7565,#5982,#5983);
#5304=AXIS2_PLACEMENT_3D('',#7566,#5984,#5985);
#5305=AXIS2_PLACEMENT_3D('',#7568,#5986,#5987);
#5306=AXIS2_PLACEMENT_3D('',#7571,#5989,#5990);
#5307=AXIS2_PLACEMENT_3D('',#7572,#5991,#5992);
#5308=AXIS2_PLACEMENT_3D('',#7573,#5993,#5994);
#5309=AXIS2_PLACEMENT_3D('',#7574,#5995,#5996);
#5310=AXIS2_PLACEMENT_3D('',#7576,#5997,#5998);
#5311=AXIS2_PLACEMENT_3D('',#7579,#6000,#6001);
#5312=AXIS2_PLACEMENT_3D('',#7580,#6002,#6003);
#5313=AXIS2_PLACEMENT_3D('',#7581,#6004,#6005);
#5314=AXIS2_PLACEMENT_3D('',#7583,#6006,#6007);
#5315=AXIS2_PLACEMENT_3D('',#7586,#6009,#6010);
#5316=AXIS2_PLACEMENT_3D('',#7587,#6011,#6012);
#5317=AXIS2_PLACEMENT_3D('',#7589,#6013,#6014);
#5318=AXIS2_PLACEMENT_3D('',#7592,#6016,#6017);
#5319=AXIS2_PLACEMENT_3D('',#7593,#6018,#6019);
#5320=AXIS2_PLACEMENT_3D('',#7595,#6020,#6021);
#5321=AXIS2_PLACEMENT_3D('',#7598,#6023,#6024);
#5322=AXIS2_PLACEMENT_3D('',#7599,#6025,#6026);
#5323=AXIS2_PLACEMENT_3D('',#7601,#6027,#6028);
#5324=AXIS2_PLACEMENT_3D('',#7604,#6030,#6031);
#5325=AXIS2_PLACEMENT_3D('',#7605,#6032,#6033);
#5326=AXIS2_PLACEMENT_3D('',#7607,#6034,#6035);
#5327=AXIS2_PLACEMENT_3D('',#7610,#6037,#6038);
#5328=AXIS2_PLACEMENT_3D('',#7611,#6039,#6040);
#5329=AXIS2_PLACEMENT_3D('',#7612,#6041,#6042);
#5330=AXIS2_PLACEMENT_3D('',#7621,#6047,#6048);
#5331=AXIS2_PLACEMENT_3D('',#7627,#6052,#6053);
#5332=AXIS2_PLACEMENT_3D('',#7633,#6057,#6058);
#5333=AXIS2_PLACEMENT_3D('',#7636,#6061,#6062);
#5334=AXIS2_PLACEMENT_3D('',#7637,#6063,#6064);
#5335=AXIS2_PLACEMENT_3D('',#7638,#6065,#6066);
#5336=AXIS2_PLACEMENT_3D('',#7639,#6067,#6068);
#5337=AXIS2_PLACEMENT_3D('',#7641,#6069,#6070);
#5338=AXIS2_PLACEMENT_3D('',#7644,#6072,#6073);
#5339=AXIS2_PLACEMENT_3D('',#7645,#6074,#6075);
#5340=AXIS2_PLACEMENT_3D('',#7654,#6080,#6081);
#5341=AXIS2_PLACEMENT_3D('',#7655,#6082,#6083);
#5342=AXIS2_PLACEMENT_3D('',#7657,#6084,#6085);
#5343=AXIS2_PLACEMENT_3D('',#7658,#6086,#6087);
#5344=AXIS2_PLACEMENT_3D('',#7659,#6088,#6089);
#5345=AXIS2_PLACEMENT_3D('',#7660,#6090,#6091);
#5346=AXIS2_PLACEMENT_3D('',#7662,#6092,#6093);
#5347=AXIS2_PLACEMENT_3D('',#7665,#6095,#6096);
#5348=AXIS2_PLACEMENT_3D('',#7666,#6097,#6098);
#5349=AXIS2_PLACEMENT_3D('',#7668,#6099,#6100);
#5350=AXIS2_PLACEMENT_3D('',#7669,#6101,#6102);
#5351=AXIS2_PLACEMENT_3D('',#7671,#6103,#6104);
#5352=AXIS2_PLACEMENT_3D('',#7672,#6105,#6106);
#5353=AXIS2_PLACEMENT_3D('',#7674,#6108,#6109);
#5354=AXIS2_PLACEMENT_3D('',#7677,#6111,#6112);
#5355=AXIS2_PLACEMENT_3D('',#7678,#6113,#6114);
#5356=AXIS2_PLACEMENT_3D('',#7680,#6115,#6116);
#5357=AXIS2_PLACEMENT_3D('',#7681,#6117,#6118);
#5358=AXIS2_PLACEMENT_3D('',#7694,#6125,#6126);
#5359=AXIS2_PLACEMENT_3D('',#7703,#6131,#6132);
#5360=AXIS2_PLACEMENT_3D('',#7710,#6137,#6138);
#5361=AXIS2_PLACEMENT_3D('',#7714,#6141,#6142);
#5362=AXIS2_PLACEMENT_3D('',#7719,#6146,#6147);
#5363=AXIS2_PLACEMENT_3D('',#7720,#6148,#6149);
#5364=AXIS2_PLACEMENT_3D('',#7726,#6153,#6154);
#5365=AXIS2_PLACEMENT_3D('',#7730,#6157,#6158);
#5366=AXIS2_PLACEMENT_3D('',#7744,#6165,#6166);
#5367=AXIS2_PLACEMENT_3D('',#7745,#6167,#6168);
#5368=AXIS2_PLACEMENT_3D('',#7748,#6171,#6172);
#5369=AXIS2_PLACEMENT_3D('',#7752,#6175,#6176);
#5370=AXIS2_PLACEMENT_3D('',#7755,#6179,#6180);
#5371=AXIS2_PLACEMENT_3D('',#7757,#6182,#6183);
#5372=AXIS2_PLACEMENT_3D('',#7759,#6185,#6186);
#5373=AXIS2_PLACEMENT_3D('',#7760,#6187,#6188);
#5374=AXIS2_PLACEMENT_3D('',#7761,#6189,#6190);
#5375=AXIS2_PLACEMENT_3D('',#7764,#6192,#6193);
#5376=AXIS2_PLACEMENT_3D('',#7765,#6194,#6195);
#5377=AXIS2_PLACEMENT_3D('',#7768,#6197,#6198);
#5378=AXIS2_PLACEMENT_3D('',#7769,#6199,#6200);
#5379=AXIS2_PLACEMENT_3D('',#7770,#6201,#6202);
#5380=AXIS2_PLACEMENT_3D('',#7771,#6203,#6204);
#5381=AXIS2_PLACEMENT_3D('',#7773,#6205,#6206);
#5382=AXIS2_PLACEMENT_3D('',#7776,#6208,#6209);
#5383=AXIS2_PLACEMENT_3D('',#7778,#6210,#6211);
#5384=AXIS2_PLACEMENT_3D('',#7780,#6213,#6214);
#5385=AXIS2_PLACEMENT_3D('',#7782,#6215,#6216);
#5386=AXIS2_PLACEMENT_3D('',#7784,#6218,#6219);
#5387=AXIS2_PLACEMENT_3D('',#7786,#6220,#6221);
#5388=AXIS2_PLACEMENT_3D('',#7787,#6222,#6223);
#5389=AXIS2_PLACEMENT_3D('',#7789,#6224,#6225);
#5390=AXIS2_PLACEMENT_3D('',#7791,#6227,#6228);
#5391=AXIS2_PLACEMENT_3D('',#7792,#6229,#6230);
#5392=AXIS2_PLACEMENT_3D('',#7793,#6231,#6232);
#5393=AXIS2_PLACEMENT_3D('',#7795,#6233,#6234);
#5394=AXIS2_PLACEMENT_3D('',#7798,#6236,#6237);
#5395=AXIS2_PLACEMENT_3D('',#7799,#6238,#6239);
#5396=AXIS2_PLACEMENT_3D('',#7800,#6240,#6241);
#5397=AXIS2_PLACEMENT_3D('',#7802,#6242,#6243);
#5398=AXIS2_PLACEMENT_3D('',#7805,#6245,#6246);
#5399=AXIS2_PLACEMENT_3D('',#7806,#6247,#6248);
#5400=AXIS2_PLACEMENT_3D('',#7807,#6249,#6250);
#5401=AXIS2_PLACEMENT_3D('',#7811,#6252,#6253);
#5402=AXIS2_PLACEMENT_3D('',#7812,#6254,#6255);
#5403=AXIS2_PLACEMENT_3D('',#7815,#6257,#6258);
#5404=AXIS2_PLACEMENT_3D('',#7816,#6259,#6260);
#5405=AXIS2_PLACEMENT_3D('',#7819,#6262,#6263);
#5406=AXIS2_PLACEMENT_3D('',#7820,#6264,#6265);
#5407=AXIS2_PLACEMENT_3D('',#7825,#6267,#6268);
#5408=AXIS2_PLACEMENT_3D('',#7829,#6270,#6271);
#5409=AXIS2_PLACEMENT_3D('',#7833,#6273,#6274);
#5410=AXIS2_PLACEMENT_3D('',#7835,#6275,#6276);
#5411=AXIS2_PLACEMENT_3D('',#7839,#6279,#6280);
#5412=AXIS2_PLACEMENT_3D('',#7840,#6281,#6282);
#5413=AXIS2_PLACEMENT_3D('',#7841,#6283,#6284);
#5414=AXIS2_PLACEMENT_3D('',#7842,#6285,#6286);
#5415=AXIS2_PLACEMENT_3D('',#7843,#6287,#6288);
#5416=AXIS2_PLACEMENT_3D('',#7844,#6289,#6290);
#5417=AXIS2_PLACEMENT_3D('',#7845,#6291,#6292);
#5418=AXIS2_PLACEMENT_3D('',#7846,#6293,#6294);
#5419=AXIS2_PLACEMENT_3D('',#7847,#6295,#6296);
#5420=AXIS2_PLACEMENT_3D('',#7848,#6297,#6298);
#5421=AXIS2_PLACEMENT_3D('',#7849,#6299,#6300);
#5422=AXIS2_PLACEMENT_3D('',#7850,#6301,#6302);
#5423=AXIS2_PLACEMENT_3D('',#7851,#6303,#6304);
#5424=AXIS2_PLACEMENT_3D('',#7852,#6305,#6306);
#5425=AXIS2_PLACEMENT_3D('',#7853,#6307,#6308);
#5426=AXIS2_PLACEMENT_3D('',#7854,#6309,#6310);
#5427=AXIS2_PLACEMENT_3D('',#7855,#6311,#6312);
#5428=AXIS2_PLACEMENT_3D('',#7856,#6313,#6314);
#5429=AXIS2_PLACEMENT_3D('',#7857,#6315,#6316);
#5430=AXIS2_PLACEMENT_3D('',#7860,#6318,#6319);
#5431=AXIS2_PLACEMENT_3D('',#7861,#6320,#6321);
#5432=AXIS2_PLACEMENT_3D('',#7863,#6322,#6323);
#5433=AXIS2_PLACEMENT_3D('',#7864,#6324,#6325);
#5434=AXIS2_PLACEMENT_3D('',#7865,#6326,#6327);
#5435=AXIS2_PLACEMENT_3D('',#7867,#6328,#6329);
#5436=AXIS2_PLACEMENT_3D('',#7870,#6331,#6332);
#5437=AXIS2_PLACEMENT_3D('',#7871,#6333,#6334);
#5438=AXIS2_PLACEMENT_3D('',#7872,#6335,#6336);
#5439=AXIS2_PLACEMENT_3D('',#7874,#6337,#6338);
#5440=AXIS2_PLACEMENT_3D('',#7877,#6340,#6341);
#5441=AXIS2_PLACEMENT_3D('',#7878,#6342,#6343);
#5442=AXIS2_PLACEMENT_3D('',#7880,#6344,#6345);
#5443=AXIS2_PLACEMENT_3D('',#7883,#6347,#6348);
#5444=AXIS2_PLACEMENT_3D('',#7884,#6349,#6350);
#5445=AXIS2_PLACEMENT_3D('',#7886,#6351,#6352);
#5446=AXIS2_PLACEMENT_3D('',#7889,#6354,#6355);
#5447=AXIS2_PLACEMENT_3D('',#7890,#6356,#6357);
#5448=AXIS2_PLACEMENT_3D('',#7892,#6358,#6359);
#5449=AXIS2_PLACEMENT_3D('',#7895,#6361,#6362);
#5450=AXIS2_PLACEMENT_3D('',#7896,#6363,#6364);
#5451=AXIS2_PLACEMENT_3D('',#7898,#6365,#6366);
#5452=AXIS2_PLACEMENT_3D('',#7900,#6368,#6369);
#5453=AXIS2_PLACEMENT_3D('',#7909,#6374,#6375);
#5454=AXIS2_PLACEMENT_3D('',#7915,#6379,#6380);
#5455=AXIS2_PLACEMENT_3D('',#7921,#6384,#6385);
#5456=AXIS2_PLACEMENT_3D('',#7924,#6388,#6389);
#5457=AXIS2_PLACEMENT_3D('',#7925,#6390,#6391);
#5458=AXIS2_PLACEMENT_3D('',#7926,#6392,#6393);
#5459=AXIS2_PLACEMENT_3D('',#7927,#6394,#6395);
#5460=AXIS2_PLACEMENT_3D('',#7929,#6396,#6397);
#5461=AXIS2_PLACEMENT_3D('',#7932,#6399,#6400);
#5462=AXIS2_PLACEMENT_3D('',#7933,#6401,#6402);
#5463=AXIS2_PLACEMENT_3D('',#7942,#6407,#6408);
#5464=AXIS2_PLACEMENT_3D('',#7943,#6409,#6410);
#5465=AXIS2_PLACEMENT_3D('',#7945,#6411,#6412);
#5466=AXIS2_PLACEMENT_3D('',#7946,#6413,#6414);
#5467=AXIS2_PLACEMENT_3D('',#7947,#6415,#6416);
#5468=AXIS2_PLACEMENT_3D('',#7948,#6417,#6418);
#5469=AXIS2_PLACEMENT_3D('',#7950,#6419,#6420);
#5470=AXIS2_PLACEMENT_3D('',#7953,#6422,#6423);
#5471=AXIS2_PLACEMENT_3D('',#7954,#6424,#6425);
#5472=AXIS2_PLACEMENT_3D('',#7956,#6426,#6427);
#5473=AXIS2_PLACEMENT_3D('',#7957,#6428,#6429);
#5474=AXIS2_PLACEMENT_3D('',#7959,#6430,#6431);
#5475=AXIS2_PLACEMENT_3D('',#7960,#6432,#6433);
#5476=AXIS2_PLACEMENT_3D('',#7962,#6435,#6436);
#5477=AXIS2_PLACEMENT_3D('',#7965,#6438,#6439);
#5478=AXIS2_PLACEMENT_3D('',#7966,#6440,#6441);
#5479=AXIS2_PLACEMENT_3D('',#7968,#6442,#6443);
#5480=AXIS2_PLACEMENT_3D('',#7969,#6444,#6445);
#5481=AXIS2_PLACEMENT_3D('',#7982,#6452,#6453);
#5482=AXIS2_PLACEMENT_3D('',#7991,#6458,#6459);
#5483=AXIS2_PLACEMENT_3D('',#7998,#6464,#6465);
#5484=AXIS2_PLACEMENT_3D('',#8002,#6468,#6469);
#5485=AXIS2_PLACEMENT_3D('',#8007,#6473,#6474);
#5486=AXIS2_PLACEMENT_3D('',#8008,#6475,#6476);
#5487=AXIS2_PLACEMENT_3D('',#8014,#6480,#6481);
#5488=AXIS2_PLACEMENT_3D('',#8018,#6484,#6485);
#5489=AXIS2_PLACEMENT_3D('',#8032,#6492,#6493);
#5490=AXIS2_PLACEMENT_3D('',#8033,#6494,#6495);
#5491=AXIS2_PLACEMENT_3D('',#8036,#6498,#6499);
#5492=AXIS2_PLACEMENT_3D('',#8040,#6502,#6503);
#5493=AXIS2_PLACEMENT_3D('',#8043,#6506,#6507);
#5494=AXIS2_PLACEMENT_3D('',#8045,#6509,#6510);
#5495=AXIS2_PLACEMENT_3D('',#8047,#6512,#6513);
#5496=AXIS2_PLACEMENT_3D('',#8048,#6514,#6515);
#5497=AXIS2_PLACEMENT_3D('',#8049,#6516,#6517);
#5498=AXIS2_PLACEMENT_3D('',#8052,#6519,#6520);
#5499=AXIS2_PLACEMENT_3D('',#8053,#6521,#6522);
#5500=AXIS2_PLACEMENT_3D('',#8056,#6524,#6525);
#5501=AXIS2_PLACEMENT_3D('',#8057,#6526,#6527);
#5502=AXIS2_PLACEMENT_3D('',#8058,#6528,#6529);
#5503=AXIS2_PLACEMENT_3D('',#8059,#6530,#6531);
#5504=AXIS2_PLACEMENT_3D('',#8061,#6532,#6533);
#5505=AXIS2_PLACEMENT_3D('',#8064,#6535,#6536);
#5506=AXIS2_PLACEMENT_3D('',#8066,#6537,#6538);
#5507=AXIS2_PLACEMENT_3D('',#8068,#6540,#6541);
#5508=AXIS2_PLACEMENT_3D('',#8070,#6542,#6543);
#5509=AXIS2_PLACEMENT_3D('',#8072,#6545,#6546);
#5510=AXIS2_PLACEMENT_3D('',#8074,#6547,#6548);
#5511=AXIS2_PLACEMENT_3D('',#8075,#6549,#6550);
#5512=AXIS2_PLACEMENT_3D('',#8077,#6551,#6552);
#5513=AXIS2_PLACEMENT_3D('',#8079,#6554,#6555);
#5514=AXIS2_PLACEMENT_3D('',#8080,#6556,#6557);
#5515=AXIS2_PLACEMENT_3D('',#8081,#6558,#6559);
#5516=AXIS2_PLACEMENT_3D('',#8083,#6560,#6561);
#5517=AXIS2_PLACEMENT_3D('',#8086,#6563,#6564);
#5518=AXIS2_PLACEMENT_3D('',#8087,#6565,#6566);
#5519=AXIS2_PLACEMENT_3D('',#8089,#6567,#6568);
#5520=AXIS2_PLACEMENT_3D('',#8092,#6570,#6571);
#5521=AXIS2_PLACEMENT_3D('',#8093,#6572,#6573);
#5522=AXIS2_PLACEMENT_3D('',#8094,#6574,#6575);
#5523=AXIS2_PLACEMENT_3D('',#8095,#6576,#6577);
#5524=AXIS2_PLACEMENT_3D('',#8096,#6578,#6579);
#5525=AXIS2_PLACEMENT_3D('',#8098,#6580,#6581);
#5526=AXIS2_PLACEMENT_3D('',#8101,#6583,#6584);
#5527=AXIS2_PLACEMENT_3D('',#8102,#6585,#6586);
#5528=AXIS2_PLACEMENT_3D('',#8104,#6587,#6588);
#5529=AXIS2_PLACEMENT_3D('',#8107,#6590,#6591);
#5530=AXIS2_PLACEMENT_3D('',#8108,#6592,#6593);
#5531=AXIS2_PLACEMENT_3D('',#8109,#6594,#6595);
#5532=AXIS2_PLACEMENT_3D('',#8110,#6596,#6597);
#5533=AXIS2_PLACEMENT_3D('',#8111,#6598,#6599);
#5534=AXIS2_PLACEMENT_3D('',#8113,#6600,#6601);
#5535=AXIS2_PLACEMENT_3D('',#8116,#6603,#6604);
#5536=AXIS2_PLACEMENT_3D('',#8117,#6605,#6606);
#5537=AXIS2_PLACEMENT_3D('',#8119,#6607,#6608);
#5538=AXIS2_PLACEMENT_3D('',#8122,#6610,#6611);
#5539=AXIS2_PLACEMENT_3D('',#8123,#6612,#6613);
#5540=AXIS2_PLACEMENT_3D('',#8124,#6614,#6615);
#5541=AXIS2_PLACEMENT_3D('',#8125,#6616,#6617);
#5542=AXIS2_PLACEMENT_3D('',#8126,#6618,#6619);
#5543=AXIS2_PLACEMENT_3D('',#8128,#6620,#6621);
#5544=AXIS2_PLACEMENT_3D('',#8131,#6623,#6624);
#5545=AXIS2_PLACEMENT_3D('',#8132,#6625,#6626);
#5546=AXIS2_PLACEMENT_3D('',#8134,#6627,#6628);
#5547=AXIS2_PLACEMENT_3D('',#8137,#6630,#6631);
#5548=AXIS2_PLACEMENT_3D('',#8138,#6632,#6633);
#5549=AXIS2_PLACEMENT_3D('',#8140,#6634,#6635);
#5550=AXIS2_PLACEMENT_3D('',#8143,#6637,#6638);
#5551=AXIS2_PLACEMENT_3D('',#8144,#6639,#6640);
#5552=AXIS2_PLACEMENT_3D('',#8146,#6641,#6642);
#5553=AXIS2_PLACEMENT_3D('',#8147,#6643,#6644);
#5554=AXIS2_PLACEMENT_3D('',#8149,#6645,#6646);
#5555=AXIS2_PLACEMENT_3D('',#8152,#6648,#6649);
#5556=AXIS2_PLACEMENT_3D('',#8153,#6650,#6651);
#5557=AXIS2_PLACEMENT_3D('',#8155,#6652,#6653);
#5558=AXIS2_PLACEMENT_3D('',#8156,#6654,#6655);
#5559=AXIS2_PLACEMENT_3D('',#8159,#6657,#6658);
#5560=AXIS2_PLACEMENT_3D('',#8160,#6659,#6660);
#5561=AXIS2_PLACEMENT_3D('',#8163,#6662,#6663);
#5562=AXIS2_PLACEMENT_3D('',#8164,#6664,#6665);
#5563=AXIS2_PLACEMENT_3D('',#8173,#6670,#6671);
#5564=AXIS2_PLACEMENT_3D('',#8179,#6675,#6676);
#5565=AXIS2_PLACEMENT_3D('',#8185,#6680,#6681);
#5566=AXIS2_PLACEMENT_3D('',#8188,#6684,#6685);
#5567=AXIS2_PLACEMENT_3D('',#8189,#6686,#6687);
#5568=AXIS2_PLACEMENT_3D('',#8190,#6688,#6689);
#5569=AXIS2_PLACEMENT_3D('',#8191,#6690,#6691);
#5570=AXIS2_PLACEMENT_3D('',#8193,#6692,#6693);
#5571=AXIS2_PLACEMENT_3D('',#8194,#6694,#6695);
#5572=AXIS2_PLACEMENT_3D('',#8196,#6696,#6697);
#5573=AXIS2_PLACEMENT_3D('',#8198,#6699,#6700);
#5574=AXIS2_PLACEMENT_3D('',#8200,#6701,#6702);
#5575=AXIS2_PLACEMENT_3D('',#8202,#6704,#6705);
#5576=AXIS2_PLACEMENT_3D('',#8204,#6706,#6707);
#5577=AXIS2_PLACEMENT_3D('',#8206,#6709,#6710);
#5578=AXIS2_PLACEMENT_3D('',#8208,#6711,#6712);
#5579=AXIS2_PLACEMENT_3D('',#8209,#6713,#6714);
#5580=AXIS2_PLACEMENT_3D('',#8211,#6715,#6716);
#5581=AXIS2_PLACEMENT_3D('',#8213,#6718,#6719);
#5582=AXIS2_PLACEMENT_3D('',#8215,#6720,#6721);
#5583=AXIS2_PLACEMENT_3D('',#8217,#6723,#6724);
#5584=AXIS2_PLACEMENT_3D('',#8219,#6725,#6726);
#5585=AXIS2_PLACEMENT_3D('',#8221,#6728,#6729);
#5586=AXIS2_PLACEMENT_3D('',#8222,#6730,#6731);
#5587=AXIS2_PLACEMENT_3D('',#8231,#6736,#6737);
#5588=AXIS2_PLACEMENT_3D('',#8237,#6741,#6742);
#5589=AXIS2_PLACEMENT_3D('',#8243,#6746,#6747);
#5590=AXIS2_PLACEMENT_3D('',#8249,#6751,#6752);
#5591=AXIS2_PLACEMENT_3D('',#8255,#6756,#6757);
#5592=AXIS2_PLACEMENT_3D('',#8258,#6760,#6761);
#5593=AXIS2_PLACEMENT_3D('',#8259,#6762,#6763);
#5594=AXIS2_PLACEMENT_3D('',#8260,#6764,#6765);
#5595=AXIS2_PLACEMENT_3D('',#8261,#6766,#6767);
#5596=AXIS2_PLACEMENT_3D('',#8262,#6768,#6769);
#5597=AXIS2_PLACEMENT_3D('',#8264,#6770,#6771);
#5598=AXIS2_PLACEMENT_3D('',#8267,#6773,#6774);
#5599=AXIS2_PLACEMENT_3D('',#8268,#6775,#6776);
#5600=AXIS2_PLACEMENT_3D('',#8270,#6777,#6778);
#5601=AXIS2_PLACEMENT_3D('',#8271,#6779,#6780);
#5602=AXIS2_PLACEMENT_3D('',#8285,#6787,#6788);
#5603=AXIS2_PLACEMENT_3D('',#8286,#6789,#6790);
#5604=AXIS2_PLACEMENT_3D('',#8300,#6797,#6798);
#5605=AXIS2_PLACEMENT_3D('',#8301,#6799,#6800);
#5606=AXIS2_PLACEMENT_3D('',#8304,#6803,#6804);
#5607=AXIS2_PLACEMENT_3D('',#8306,#6806,#6807);
#5608=AXIS2_PLACEMENT_3D('',#8308,#6809,#6810);
#5609=AXIS2_PLACEMENT_3D('',#8310,#6812,#6813);
#5610=AXIS2_PLACEMENT_3D('',#8312,#6815,#6816);
#5611=AXIS2_PLACEMENT_3D('',#8313,#6817,#6818);
#5612=AXIS2_PLACEMENT_3D('',#8315,#6819,#6820);
#5613=AXIS2_PLACEMENT_3D('',#8316,#6821,#6822);
#5614=AXIS2_PLACEMENT_3D('',#8319,#6824,#6825);
#5615=AXIS2_PLACEMENT_3D('',#8320,#6826,#6827);
#5616=AXIS2_PLACEMENT_3D('',#8322,#6828,#6829);
#5617=AXIS2_PLACEMENT_3D('',#8323,#6830,#6831);
#5618=AXIS2_PLACEMENT_3D('',#8325,#6833,#6834);
#5619=AXIS2_PLACEMENT_3D('',#8327,#6835,#6836);
#5620=AXIS2_PLACEMENT_3D('',#8329,#6838,#6839);
#5621=AXIS2_PLACEMENT_3D('',#8331,#6840,#6841);
#5622=AXIS2_PLACEMENT_3D('',#8332,#6842,#6843);
#5623=AXIS2_PLACEMENT_3D('',#8334,#6845,#6846);
#5624=AXIS2_PLACEMENT_3D('',#8335,#6847,#6848);
#5625=AXIS2_PLACEMENT_3D('',#8337,#6849,#6850);
#5626=AXIS2_PLACEMENT_3D('',#8339,#6851,#6852);
#5627=AXIS2_PLACEMENT_3D('',#8340,#6853,#6854);
#5628=AXIS2_PLACEMENT_3D('',#8342,#6855,#6856);
#5629=AXIS2_PLACEMENT_3D('',#8344,#6858,#6859);
#5630=AXIS2_PLACEMENT_3D('',#8346,#6860,#6861);
#5631=AXIS2_PLACEMENT_3D('',#8347,#6862,#6863);
#5632=AXIS2_PLACEMENT_3D('',#8349,#6864,#6865);
#5633=AXIS2_PLACEMENT_3D('',#8351,#6867,#6868);
#5634=AXIS2_PLACEMENT_3D('',#8353,#6869,#6870);
#5635=AXIS2_PLACEMENT_3D('',#8354,#6871,#6872);
#5636=AXIS2_PLACEMENT_3D('',#8356,#6874,#6875);
#5637=AXIS2_PLACEMENT_3D('',#8357,#6876,#6877);
#5638=AXIS2_PLACEMENT_3D('',#8358,#6878,#6879);
#5639=AXIS2_PLACEMENT_3D('',#8359,#6880,#6881);
#5640=AXIS2_PLACEMENT_3D('',#8361,#6882,#6883);
#5641=AXIS2_PLACEMENT_3D('',#8362,#6884,#6885);
#5642=AXIS2_PLACEMENT_3D('',#8363,#6886,#6887);
#5643=AXIS2_PLACEMENT_3D('',#8364,#6888,#6889);
#5644=AXIS2_PLACEMENT_3D('',#8366,#6890,#6891);
#5645=AXIS2_PLACEMENT_3D('',#8369,#6893,#6894);
#5646=AXIS2_PLACEMENT_3D('',#8370,#6895,#6896);
#5647=AXIS2_PLACEMENT_3D('',#8372,#6897,#6898);
#5648=AXIS2_PLACEMENT_3D('',#8373,#6899,#6900);
#5649=AXIS2_PLACEMENT_3D('',#8375,#6901,#6902);
#5650=AXIS2_PLACEMENT_3D('',#8376,#6903,#6904);
#5651=AXIS2_PLACEMENT_3D('',#8379,#6906,#6907);
#5652=AXIS2_PLACEMENT_3D('',#8380,#6908,#6909);
#5653=AXIS2_PLACEMENT_3D('',#8382,#6910,#6911);
#5654=AXIS2_PLACEMENT_3D('',#8384,#6913,#6914);
#5655=AXIS2_PLACEMENT_3D('',#8386,#6915,#6916);
#5656=AXIS2_PLACEMENT_3D('',#8389,#6918,#6919);
#5657=AXIS2_PLACEMENT_3D('',#8390,#6920,#6921);
#5658=AXIS2_PLACEMENT_3D('',#8391,#6922,#6923);
#5659=AXIS2_PLACEMENT_3D('',#8392,#6924,#6925);
#5660=AXIS2_PLACEMENT_3D('',#8393,#6926,#6927);
#5661=AXIS2_PLACEMENT_3D('',#8395,#6928,#6929);
#5662=AXIS2_PLACEMENT_3D('',#8396,#6930,#6931);
#5663=AXIS2_PLACEMENT_3D('',#8397,#6932,#6933);
#5664=AXIS2_PLACEMENT_3D('',#8398,#6934,#6935);
#5665=AXIS2_PLACEMENT_3D('',#8400,#6936,#6937);
#5666=AXIS2_PLACEMENT_3D('',#8403,#6939,#6940);
#5667=AXIS2_PLACEMENT_3D('',#8404,#6941,#6942);
#5668=AXIS2_PLACEMENT_3D('',#8405,#6943,#6944);
#5669=AXIS2_PLACEMENT_3D('',#8406,#6945,#6946);
#5670=AXIS2_PLACEMENT_3D('',#8407,#6947,#6948);
#5671=AXIS2_PLACEMENT_3D('',#8409,#6949,#6950);
#5672=AXIS2_PLACEMENT_3D('',#8412,#6952,#6953);
#5673=AXIS2_PLACEMENT_3D('',#8413,#6954,#6955);
#5674=AXIS2_PLACEMENT_3D('',#8416,#6957,#6958);
#5675=AXIS2_PLACEMENT_3D('',#8417,#6959,#6960);
#5676=AXIS2_PLACEMENT_3D('',#8419,#6961,#6962);
#5677=AXIS2_PLACEMENT_3D('',#8420,#6963,#6964);
#5678=AXIS2_PLACEMENT_3D('',#8423,#6966,#6967);
#5679=AXIS2_PLACEMENT_3D('',#8424,#6968,#6969);
#5680=AXIS2_PLACEMENT_3D('',#8425,#6970,#6971);
#5681=AXIS2_PLACEMENT_3D('',#8426,#6972,#6973);
#5682=AXIS2_PLACEMENT_3D('',#8438,#6975,#6976);
#5683=AXIS2_PLACEMENT_3D('',#8454,#6977,#6978);
#5684=AXIS2_PLACEMENT_3D('',#8456,#6979,#6980);
#5685=AXIS2_PLACEMENT_3D('',#8482,#6982,#6983);
#5686=AXIS2_PLACEMENT_3D('',#8485,#6986,#6987);
#5687=AXIS2_PLACEMENT_3D('',#8487,#6989,#6990);
#5688=AXIS2_PLACEMENT_3D('',#8489,#6992,#6993);
#5689=AXIS2_PLACEMENT_3D('',#8491,#6994,#6995);
#5690=AXIS2_PLACEMENT_3D('',#8494,#6997,#6998);
#5691=AXIS2_PLACEMENT_3D('',#8495,#6999,#7000);
#5692=AXIS2_PLACEMENT_3D('',#8497,#7002,#7003);
#5693=AXIS2_PLACEMENT_3D('',#8499,#7005,#7006);
#5694=AXIS2_PLACEMENT_3D('',#8500,#7007,#7008);
#5695=AXIS2_PLACEMENT_3D('',#8501,#7009,#7010);
#5696=AXIS2_PLACEMENT_3D('',#8502,#7011,#7012);
#5697=AXIS2_PLACEMENT_3D('',#8503,#7013,#7014);
#5698=AXIS2_PLACEMENT_3D('',#8504,#7015,#7016);
#5699=AXIS2_PLACEMENT_3D('',#8505,#7017,#7018);
#5700=AXIS2_PLACEMENT_3D('',#8506,#7019,#7020);
#5701=AXIS2_PLACEMENT_3D('',#8507,#7021,#7022);
#5702=AXIS2_PLACEMENT_3D('',#8508,#7023,#7024);
#5703=AXIS2_PLACEMENT_3D('',#8509,#7025,#7026);
#5704=AXIS2_PLACEMENT_3D('',#8510,#7027,#7028);
#5705=AXIS2_PLACEMENT_3D('',#8511,#7029,#7030);
#5706=AXIS2_PLACEMENT_3D('',#8512,#7031,#7032);
#5707=AXIS2_PLACEMENT_3D('',#8513,#7033,#7034);
#5708=AXIS2_PLACEMENT_3D('',#8514,#7035,#7036);
#5709=AXIS2_PLACEMENT_3D('',#8515,#7037,#7038);
#5710=AXIS2_PLACEMENT_3D('',#8516,#7039,#7040);
#5711=AXIS2_PLACEMENT_3D('',#8517,#7041,#7042);
#5712=AXIS2_PLACEMENT_3D('',#8518,#7043,#7044);
#5713=AXIS2_PLACEMENT_3D('',#8519,#7045,#7046);
#5714=AXIS2_PLACEMENT_3D('',#8520,#7047,#7048);
#5715=AXIS2_PLACEMENT_3D('',#8521,#7049,#7050);
#5716=AXIS2_PLACEMENT_3D('',#8522,#7051,#7052);
#5717=AXIS2_PLACEMENT_3D('',#8523,#7053,#7054);
#5718=AXIS2_PLACEMENT_3D('',#8524,#7055,#7056);
#5719=AXIS2_PLACEMENT_3D('',#8525,#7057,#7058);
#5720=AXIS2_PLACEMENT_3D('',#8526,#7059,#7060);
#5721=AXIS2_PLACEMENT_3D('',#8527,#7061,#7062);
#5722=AXIS2_PLACEMENT_3D('',#8528,#7063,#7064);
#5723=AXIS2_PLACEMENT_3D('',#8529,#7065,#7066);
#5724=AXIS2_PLACEMENT_3D('',#8530,#7067,#7068);
#5725=AXIS2_PLACEMENT_3D('',#8531,#7069,#7070);
#5726=AXIS2_PLACEMENT_3D('',#8532,#7071,#7072);
#5727=AXIS2_PLACEMENT_3D('',#8533,#7073,#7074);
#5728=AXIS2_PLACEMENT_3D('',#8534,#7075,#7076);
#5729=AXIS2_PLACEMENT_3D('',#8535,#7077,#7078);
#5730=AXIS2_PLACEMENT_3D('',#8536,#7079,#7080);
#5731=AXIS2_PLACEMENT_3D('',#8537,#7081,#7082);
#5732=AXIS2_PLACEMENT_3D('',#8538,#7083,#7084);
#5733=AXIS2_PLACEMENT_3D('',#8539,#7085,#7086);
#5734=AXIS2_PLACEMENT_3D('',#8540,#7087,#7088);
#5735=AXIS2_PLACEMENT_3D('',#8541,#7089,#7090);
#5736=AXIS2_PLACEMENT_3D('',#8542,#7091,#7092);
#5737=AXIS2_PLACEMENT_3D('',#8543,#7093,#7094);
#5738=AXIS2_PLACEMENT_3D('',#8544,#7095,#7096);
#5739=AXIS2_PLACEMENT_3D('',#8545,#7097,#7098);
#5740=AXIS2_PLACEMENT_3D('',#8547,#7099,#7100);
#5741=AXIS2_PLACEMENT_3D('',#8550,#7102,#7103);
#5742=AXIS2_PLACEMENT_3D('',#8551,#7104,#7105);
#5743=AXIS2_PLACEMENT_3D('',#8553,#7106,#7107);
#5744=AXIS2_PLACEMENT_3D('',#8554,#7108,#7109);
#5745=AXIS2_PLACEMENT_3D('',#8556,#7110,#7111);
#5746=AXIS2_PLACEMENT_3D('',#8559,#7113,#7114);
#5747=AXIS2_PLACEMENT_3D('',#8560,#7115,#7116);
#5748=AXIS2_PLACEMENT_3D('',#8562,#7117,#7118);
#5749=AXIS2_PLACEMENT_3D('',#8563,#7119,#7120);
#5750=AXIS2_PLACEMENT_3D('',#8565,#7121,#7122);
#5751=AXIS2_PLACEMENT_3D('',#8566,#7123,#7124);
#5752=AXIS2_PLACEMENT_3D('',#8569,#7126,#7127);
#5753=AXIS2_PLACEMENT_3D('',#8570,#7128,#7129);
#5754=AXIS2_PLACEMENT_3D('',#8573,#7131,#7132);
#5755=AXIS2_PLACEMENT_3D('',#8574,#7133,#7134);
#5756=AXIS2_PLACEMENT_3D('',#8576,#7135,#7136);
#5757=AXIS2_PLACEMENT_3D('',#8578,#7138,#7139);
#5758=AXIS2_PLACEMENT_3D('',#8579,#7140,#7141);
#5759=AXIS2_PLACEMENT_3D('',#8580,#7142,#7143);
#5760=AXIS2_PLACEMENT_3D('',#8581,#7144,#7145);
#5761=AXIS2_PLACEMENT_3D('',#8583,#7146,#7147);
#5762=AXIS2_PLACEMENT_3D('',#8584,#7148,#7149);
#5763=AXIS2_PLACEMENT_3D('',#8585,#7150,#7151);
#5764=AXIS2_PLACEMENT_3D('',#8586,#7152,#7153);
#5765=AXIS2_PLACEMENT_3D('',#8588,#7154,#7155);
#5766=AXIS2_PLACEMENT_3D('',#8591,#7157,#7158);
#5767=AXIS2_PLACEMENT_3D('',#8592,#7159,#7160);
#5768=AXIS2_PLACEMENT_3D('',#8593,#7161,#7162);
#5769=AXIS2_PLACEMENT_3D('',#8595,#7163,#7164);
#5770=AXIS2_PLACEMENT_3D('',#8598,#7166,#7167);
#5771=AXIS2_PLACEMENT_3D('',#8599,#7168,#7169);
#5772=AXIS2_PLACEMENT_3D('',#8600,#7170,#7171);
#5773=AXIS2_PLACEMENT_3D('',#8601,#7172,#7173);
#5774=AXIS2_PLACEMENT_3D('',#8602,#7174,#7175);
#5775=AXIS2_PLACEMENT_3D('',#8604,#7176,#7177);
#5776=AXIS2_PLACEMENT_3D('',#8605,#7178,#7179);
#5777=AXIS2_PLACEMENT_3D('',#8607,#7180,#7181);
#5778=AXIS2_PLACEMENT_3D('',#8609,#7183,#7184);
#5779=AXIS2_PLACEMENT_3D('',#8611,#7185,#7186);
#5780=AXIS2_PLACEMENT_3D('',#8613,#7188,#7189);
#5781=AXIS2_PLACEMENT_3D('',#8615,#7190,#7191);
#5782=AXIS2_PLACEMENT_3D('',#8617,#7193,#7194);
#5783=AXIS2_PLACEMENT_3D('',#8619,#7195,#7196);
#5784=AXIS2_PLACEMENT_3D('',#8620,#7197,#7198);
#5785=AXIS2_PLACEMENT_3D('',#8622,#7199,#7200);
#5786=AXIS2_PLACEMENT_3D('',#8624,#7202,#7203);
#5787=AXIS2_PLACEMENT_3D('',#8626,#7204,#7205);
#5788=AXIS2_PLACEMENT_3D('',#8628,#7207,#7208);
#5789=AXIS2_PLACEMENT_3D('',#8630,#7209,#7210);
#5790=AXIS2_PLACEMENT_3D('',#8632,#7212,#7213);
#5791=AXIS2_PLACEMENT_3D('',#8633,#7214,#7215);
#5792=AXIS2_PLACEMENT_3D('',#8642,#7220,#7221);
#5793=AXIS2_PLACEMENT_3D('',#8648,#7225,#7226);
#5794=AXIS2_PLACEMENT_3D('',#8654,#7230,#7231);
#5795=AXIS2_PLACEMENT_3D('',#8660,#7235,#7236);
#5796=AXIS2_PLACEMENT_3D('',#8666,#7240,#7241);
#5797=AXIS2_PLACEMENT_3D('',#8669,#7244,#7245);
#5798=AXIS2_PLACEMENT_3D('',#8670,#7246,#7247);
#5799=AXIS2_PLACEMENT_3D('',#8671,#7248,#7249);
#5800=AXIS2_PLACEMENT_3D('',#8672,#7250,#7251);
#5801=AXIS2_PLACEMENT_3D('',#8674,#7252,#7253);
#5802=AXIS2_PLACEMENT_3D('',#8677,#7255,#7256);
#5803=AXIS2_PLACEMENT_3D('',#8678,#7257,#7258);
#5804=AXIS2_PLACEMENT_3D('',#8680,#7259,#7260);
#5805=AXIS2_PLACEMENT_3D('',#8683,#7262,#7263);
#5806=AXIS2_PLACEMENT_3D('',#8684,#7264,#7265);
#5807=AXIS2_PLACEMENT_3D('',#8688,#7267,#7268);
#5808=AXIS2_PLACEMENT_3D('',#8689,#7269,#7270);
#5809=AXIS2_PLACEMENT_3D('',#8702,#7271,#7272);
#5810=AXIS2_PLACEMENT_3D('',#8705,#7274,#7275);
#5811=AXIS2_PLACEMENT_3D('',#8707,#7276,#7277);
#5812=AXIS2_PLACEMENT_3D('',#8718,#7278,#7279);
#5813=AXIS2_PLACEMENT_3D('',#8720,#7281,#7282);
#5814=AXIS2_PLACEMENT_3D('',#8722,#7283,#7284);
#5815=AXIS2_PLACEMENT_3D('',#8725,#7286,#7287);
#5816=AXIS2_PLACEMENT_3D('',#8726,#7288,#7289);
#5817=AXIS2_PLACEMENT_3D('',#8735,#7294,#7295);
#5818=AXIS2_PLACEMENT_3D('',#8741,#7299,#7300);
#5819=AXIS2_PLACEMENT_3D('',#8747,#7304,#7305);
#5820=AXIS2_PLACEMENT_3D('',#8757,#7311,#7312);
#5821=AXIS2_PLACEMENT_3D('',#8761,#7315,#7316);
#5822=AXIS2_PLACEMENT_3D('',#8765,#7319,#7320);
#5823=AXIS2_PLACEMENT_3D('',#8771,#7324,#7325);
#5824=AXIS2_PLACEMENT_3D('',#8773,#7327,#7328);
#5825=AXIS2_PLACEMENT_3D('',#8775,#7330,#7331);
#5826=AXIS2_PLACEMENT_3D('',#8776,#7332,#7333);
#5827=AXIS2_PLACEMENT_3D('',#8777,#7334,#7335);
#5828=AXIS2_PLACEMENT_3D('',#8786,#7340,#7341);
#5829=AXIS2_PLACEMENT_3D('',#8792,#7345,#7346);
#5830=AXIS2_PLACEMENT_3D('',#8798,#7350,#7351);
#5831=AXIS2_PLACEMENT_3D('',#8804,#7355,#7356);
#5832=AXIS2_PLACEMENT_3D('',#8810,#7360,#7361);
#5833=AXIS2_PLACEMENT_3D('',#8813,#7364,#7365);
#5834=AXIS2_PLACEMENT_3D('',#8814,#7366,#7367);
#5835=AXIS2_PLACEMENT_3D('',#8816,#7368,#7369);
#5836=AXIS2_PLACEMENT_3D('',#8817,#7370,#7371);
#5837=AXIS2_PLACEMENT_3D('',#8819,#7372,#7373);
#5838=AXIS2_PLACEMENT_3D('',#8821,#7375,#7376);
#5839=AXIS2_PLACEMENT_3D('',#8823,#7377,#7378);
#5840=AXIS2_PLACEMENT_3D('',#8825,#7380,#7381);
#5841=AXIS2_PLACEMENT_3D('',#8827,#7382,#7383);
#5842=AXIS2_PLACEMENT_3D('',#8829,#7385,#7386);
#5843=AXIS2_PLACEMENT_3D('',#8830,#7387,#7388);
#5844=AXIS2_PLACEMENT_3D('',#8831,#7389,#7390);
#5845=AXIS2_PLACEMENT_3D('',#8909,#7392,#7393);
#5846=AXIS2_PLACEMENT_3D('',#8911,#7394,#7395);
#5847=AXIS2_PLACEMENT_3D('',#8912,#7396,#7397);
#5848=AXIS2_PLACEMENT_3D('',#8914,#7398,#7399);
#5849=AXIS2_PLACEMENT_3D('',#8916,#7401,#7402);
#5850=AXIS2_PLACEMENT_3D('',#8918,#7403,#7404);
#5851=AXIS2_PLACEMENT_3D('',#8920,#7406,#7407);
#5852=AXIS2_PLACEMENT_3D('',#8922,#7408,#7409);
#5853=AXIS2_PLACEMENT_3D('',#8923,#7410,#7411);
#5854=AXIS2_PLACEMENT_3D('',#8925,#7412,#7413);
#5855=AXIS2_PLACEMENT_3D('',#8928,#7416,#7417);
#5856=AXIS2_PLACEMENT_3D('',#8930,#7418,#7419);
#5857=AXIS2_PLACEMENT_3D('',#8932,#7421,#7422);
#5858=AXIS2_PLACEMENT_3D('',#8933,#7423,#7424);
#5859=AXIS2_PLACEMENT_3D('',#8934,#7425,#7426);
#5860=AXIS2_PLACEMENT_3D('',#8936,#7427,#7428);
#5861=AXIS2_PLACEMENT_3D('',#8939,#7430,#7431);
#5862=AXIS2_PLACEMENT_3D('',#8940,#7432,#7433);
#5863=AXIS2_PLACEMENT_3D('',#8942,#7434,#7435);
#5864=AXIS2_PLACEMENT_3D('',#8945,#7437,#7438);
#5865=AXIS2_PLACEMENT_3D('',#8946,#7439,#7440);
#5866=AXIS2_PLACEMENT_3D('',#8947,#7441,#7442);
#5867=AXIS2_PLACEMENT_3D('',#8948,#7443,#7444);
#5868=AXIS2_PLACEMENT_3D('',#8949,#7445,#7446);
#5869=AXIS2_PLACEMENT_3D('',#8951,#7447,#7448);
#5870=AXIS2_PLACEMENT_3D('',#8952,#7449,#7450);
#5871=AXIS2_PLACEMENT_3D('',#9007,#7451,#7452);
#5872=AXIS2_PLACEMENT_3D('',#9010,#7453,#7454);
#5873=AXIS2_PLACEMENT_3D('',#9012,#7456,#7457);
#5874=AXIS2_PLACEMENT_3D('',#9018,#7461,#7462);
#5875=AXIS2_PLACEMENT_3D('',#9020,#7463,#7464);
#5876=AXIS2_PLACEMENT_3D('',#9022,#7466,#7467);
#5877=AXIS2_PLACEMENT_3D('',#9023,#7468,#7469);
#5878=AXIS2_PLACEMENT_3D('',#9024,#7470,#7471);
#5879=AXIS2_PLACEMENT_3D('',#9025,#7472,#7473);
#5880=AXIS2_PLACEMENT_3D('',#9026,#7474,#7475);
#5881=AXIS2_PLACEMENT_3D('',#9027,#7476,#7477);
#5882=AXIS2_PLACEMENT_3D('',#9028,#7478,#7479);
#5883=AXIS2_PLACEMENT_3D('',#9029,#7480,#7481);
#5884=AXIS2_PLACEMENT_3D('',#9030,#7482,#7483);
#5885=AXIS2_PLACEMENT_3D('',#9031,#7484,#7485);
#5886=AXIS2_PLACEMENT_3D('',#9032,#7486,#7487);
#5887=AXIS2_PLACEMENT_3D('',#9033,#7488,#7489);
#5888=AXIS2_PLACEMENT_3D('',#9034,#7490,#7491);
#5889=AXIS2_PLACEMENT_3D('',#9035,#7492,#7493);
#5890=AXIS2_PLACEMENT_3D('',#9036,#7494,#7495);
#5891=DIRECTION('axis',(0.,0.,1.));
#5892=DIRECTION('refdir',(1.,0.,0.));
#5893=DIRECTION('axis',(0.,0.,1.));
#5894=DIRECTION('refdir',(1.,0.,0.));
#5895=DIRECTION('axis',(0.,0.,1.));
#5896=DIRECTION('refdir',(1.,0.,0.));
#5897=DIRECTION('center_axis',(0.,0.,1.));
#5898=DIRECTION('ref_axis',(1.,0.,0.));
#5899=DIRECTION('center_axis',(0.,0.,1.));
#5900=DIRECTION('ref_axis',(1.,0.,0.));
#5901=DIRECTION('',(0.,0.,1.));
#5902=DIRECTION('center_axis',(0.,0.,1.));
#5903=DIRECTION('ref_axis',(1.,0.,0.));
#5904=DIRECTION('center_axis',(0.,0.,1.));
#5905=DIRECTION('ref_axis',(1.,0.,0.));
#5906=DIRECTION('center_axis',(0.,0.,1.));
#5907=DIRECTION('ref_axis',(1.,0.,0.));
#5908=DIRECTION('center_axis',(0.,0.,1.));
#5909=DIRECTION('ref_axis',(1.,0.,0.));
#5910=DIRECTION('',(0.,0.,1.));
#5911=DIRECTION('center_axis',(0.,0.,1.));
#5912=DIRECTION('ref_axis',(1.,0.,0.));
#5913=DIRECTION('center_axis',(0.,0.,1.));
#5914=DIRECTION('ref_axis',(1.,0.,0.));
#5915=DIRECTION('center_axis',(0.,1.,0.));
#5916=DIRECTION('ref_axis',(1.,0.,0.));
#5917=DIRECTION('',(-1.,0.,0.));
#5918=DIRECTION('center_axis',(0.,1.,0.));
#5919=DIRECTION('ref_axis',(1.,0.,0.));
#5920=DIRECTION('center_axis',(0.,1.,0.));
#5921=DIRECTION('ref_axis',(1.,0.,0.));
#5922=DIRECTION('',(0.,0.,-1.));
#5923=DIRECTION('center_axis',(0.,1.,0.));
#5924=DIRECTION('ref_axis',(1.,0.,0.));
#5925=DIRECTION('center_axis',(0.,1.,0.));
#5926=DIRECTION('ref_axis',(1.,0.,0.));
#5927=DIRECTION('center_axis',(0.,-0.707106781186548,-0.707106781186547));
#5928=DIRECTION('ref_axis',(0.,0.707106781186547,-0.707106781186548));
#5929=DIRECTION('center_axis',(0.,-0.707106781186548,0.707106781186547));
#5930=DIRECTION('ref_axis',(0.,-0.707106781186547,-0.707106781186548));
#5931=DIRECTION('center_axis',(0.,1.,0.));
#5932=DIRECTION('ref_axis',(1.,0.,0.));
#5933=DIRECTION('',(0.,1.,0.));
#5934=DIRECTION('',(0.,-1.,0.));
#5935=DIRECTION('center_axis',(0.,0.707106781186548,0.707106781186547));
#5936=DIRECTION('ref_axis',(0.,0.707106781186547,-0.707106781186548));
#5937=DIRECTION('center_axis',(0.,0.707106781186548,-0.707106781186547));
#5938=DIRECTION('ref_axis',(0.,-0.707106781186547,-0.707106781186548));
#5939=DIRECTION('',(0.,1.,0.));
#5940=DIRECTION('center_axis',(0.,-1.,0.));
#5941=DIRECTION('ref_axis',(1.,0.,0.));
#5942=DIRECTION('',(0.,-1.,0.));
#5943=DIRECTION('center_axis',(0.,1.,0.));
#5944=DIRECTION('ref_axis',(1.,0.,0.));
#5945=DIRECTION('',(0.,1.,0.));
#5946=DIRECTION('center_axis',(0.,-1.,0.));
#5947=DIRECTION('ref_axis',(1.,0.,0.));
#5948=DIRECTION('center_axis',(0.,0.707106781186548,0.707106781186547));
#5949=DIRECTION('ref_axis',(0.,0.707106781186547,-0.707106781186548));
#5950=DIRECTION('center_axis',(0.,1.,0.));
#5951=DIRECTION('ref_axis',(-1.,0.,-2.54207057918564E-15));
#5952=DIRECTION('center_axis',(0.,-0.707106781186548,-0.707106781186547));
#5953=DIRECTION('ref_axis',(0.,0.707106781186547,-0.707106781186548));
#5954=DIRECTION('center_axis',(0.,1.,0.));
#5955=DIRECTION('ref_axis',(1.,0.,0.));
#5956=DIRECTION('center_axis',(0.,-0.707106781186548,0.707106781186547));
#5957=DIRECTION('ref_axis',(0.,-0.707106781186547,-0.707106781186548));
#5958=DIRECTION('center_axis',(0.,1.,0.));
#5959=DIRECTION('ref_axis',(1.,0.,0.));
#5960=DIRECTION('center_axis',(0.,-1.,0.));
#5961=DIRECTION('ref_axis',(1.,0.,0.));
#5962=DIRECTION('center_axis',(0.,1.,0.));
#5963=DIRECTION('ref_axis',(1.,0.,0.));
#5964=DIRECTION('',(0.,0.,1.));
#5965=DIRECTION('center_axis',(0.,0.,1.));
#5966=DIRECTION('ref_axis',(1.,0.,0.));
#5967=DIRECTION('center_axis',(0.,0.,1.));
#5968=DIRECTION('ref_axis',(1.,0.,0.));
#5969=DIRECTION('center_axis',(0.,0.,1.));
#5970=DIRECTION('ref_axis',(1.,0.,0.));
#5971=DIRECTION('center_axis',(0.,0.,1.));
#5972=DIRECTION('ref_axis',(1.,0.,0.));
#5973=DIRECTION('center_axis',(0.,0.,1.));
#5974=DIRECTION('ref_axis',(1.,0.,0.));
#5975=DIRECTION('center_axis',(0.,0.,1.));
#5976=DIRECTION('ref_axis',(1.,0.,0.));
#5977=DIRECTION('',(0.,0.,1.));
#5978=DIRECTION('center_axis',(0.,0.,-1.));
#5979=DIRECTION('ref_axis',(1.,0.,0.));
#5980=DIRECTION('center_axis',(0.,0.,1.));
#5981=DIRECTION('ref_axis',(-1.,-1.65389215948552E-15,0.));
#5982=DIRECTION('center_axis',(0.,0.,1.));
#5983=DIRECTION('ref_axis',(1.,0.,0.));
#5984=DIRECTION('center_axis',(0.,1.,0.));
#5985=DIRECTION('ref_axis',(1.,0.,0.));
#5986=DIRECTION('center_axis',(0.,1.,0.));
#5987=DIRECTION('ref_axis',(1.,0.,0.));
#5988=DIRECTION('',(0.,1.,0.));
#5989=DIRECTION('center_axis',(0.,-1.,0.));
#5990=DIRECTION('ref_axis',(1.,0.,0.));
#5991=DIRECTION('center_axis',(0.,1.,0.));
#5992=DIRECTION('ref_axis',(1.,0.,0.));
#5993=DIRECTION('center_axis',(0.,0.,1.));
#5994=DIRECTION('ref_axis',(1.,0.,0.));
#5995=DIRECTION('center_axis',(0.,0.,1.));
#5996=DIRECTION('ref_axis',(1.,0.,0.));
#5997=DIRECTION('center_axis',(0.,0.,1.));
#5998=DIRECTION('ref_axis',(1.,0.,0.));
#5999=DIRECTION('',(0.,0.,1.));
#6000=DIRECTION('center_axis',(0.,0.,-1.));
#6001=DIRECTION('ref_axis',(1.,0.,0.));
#6002=DIRECTION('center_axis',(0.,0.,1.));
#6003=DIRECTION('ref_axis',(1.,0.,0.));
#6004=DIRECTION('center_axis',(0.,1.,0.));
#6005=DIRECTION('ref_axis',(1.,0.,0.));
#6006=DIRECTION('center_axis',(0.,1.,0.));
#6007=DIRECTION('ref_axis',(1.,0.,0.));
#6008=DIRECTION('',(0.,1.,0.));
#6009=DIRECTION('center_axis',(0.,-1.,0.));
#6010=DIRECTION('ref_axis',(1.,0.,0.));
#6011=DIRECTION('center_axis',(0.,1.,0.));
#6012=DIRECTION('ref_axis',(1.,0.,0.));
#6013=DIRECTION('center_axis',(0.,1.,0.));
#6014=DIRECTION('ref_axis',(1.,0.,0.));
#6015=DIRECTION('',(0.,1.,0.));
#6016=DIRECTION('center_axis',(0.,-1.,0.));
#6017=DIRECTION('ref_axis',(1.,0.,0.));
#6018=DIRECTION('center_axis',(0.,1.,0.));
#6019=DIRECTION('ref_axis',(1.,0.,0.));
#6020=DIRECTION('center_axis',(0.,1.,0.));
#6021=DIRECTION('ref_axis',(1.,0.,0.));
#6022=DIRECTION('',(0.,1.,0.));
#6023=DIRECTION('center_axis',(0.,-1.,0.));
#6024=DIRECTION('ref_axis',(1.,0.,0.));
#6025=DIRECTION('center_axis',(0.,1.,0.));
#6026=DIRECTION('ref_axis',(1.,0.,0.));
#6027=DIRECTION('center_axis',(0.,1.,0.));
#6028=DIRECTION('ref_axis',(1.,0.,0.));
#6029=DIRECTION('',(0.,1.,0.));
#6030=DIRECTION('center_axis',(0.,-1.,0.));
#6031=DIRECTION('ref_axis',(1.,0.,0.));
#6032=DIRECTION('center_axis',(0.,1.,0.));
#6033=DIRECTION('ref_axis',(1.,0.,0.));
#6034=DIRECTION('center_axis',(0.,1.,0.));
#6035=DIRECTION('ref_axis',(1.,0.,0.));
#6036=DIRECTION('',(0.,1.,0.));
#6037=DIRECTION('center_axis',(0.,-1.,0.));
#6038=DIRECTION('ref_axis',(1.,0.,0.));
#6039=DIRECTION('center_axis',(0.,1.,0.));
#6040=DIRECTION('ref_axis',(1.,0.,0.));
#6041=DIRECTION('center_axis',(0.,1.,0.));
#6042=DIRECTION('ref_axis',(-1.,0.,0.));
#6043=DIRECTION('',(-1.,0.,0.));
#6044=DIRECTION('',(0.,0.,1.));
#6045=DIRECTION('',(-1.,0.,0.));
#6046=DIRECTION('',(0.,0.,1.));
#6047=DIRECTION('center_axis',(1.,0.,0.));
#6048=DIRECTION('ref_axis',(0.,1.,0.));
#6049=DIRECTION('',(0.,1.,0.));
#6050=DIRECTION('',(0.,1.,0.));
#6051=DIRECTION('',(0.,0.,1.));
#6052=DIRECTION('center_axis',(0.,-1.,0.));
#6053=DIRECTION('ref_axis',(1.,0.,0.));
#6054=DIRECTION('',(1.,0.,0.));
#6055=DIRECTION('',(1.,0.,0.));
#6056=DIRECTION('',(0.,0.,1.));
#6057=DIRECTION('center_axis',(-1.,0.,0.));
#6058=DIRECTION('ref_axis',(0.,-1.,0.));
#6059=DIRECTION('',(0.,-1.,0.));
#6060=DIRECTION('',(0.,-1.,0.));
#6061=DIRECTION('center_axis',(0.,0.,1.));
#6062=DIRECTION('ref_axis',(1.,0.,0.));
#6063=DIRECTION('center_axis',(0.,0.,1.));
#6064=DIRECTION('ref_axis',(1.,0.,0.));
#6065=DIRECTION('axis',(0.,0.,1.));
#6066=DIRECTION('refdir',(1.,0.,0.));
#6067=DIRECTION('center_axis',(1.,0.,0.));
#6068=DIRECTION('ref_axis',(0.,0.,-1.));
#6069=DIRECTION('center_axis',(1.,0.,0.));
#6070=DIRECTION('ref_axis',(0.,0.,-1.));
#6071=DIRECTION('',(1.,0.,0.));
#6072=DIRECTION('center_axis',(-1.,0.,0.));
#6073=DIRECTION('ref_axis',(0.,0.,-1.));
#6074=DIRECTION('center_axis',(1.,0.,0.));
#6075=DIRECTION('ref_axis',(0.,0.,-1.));
#6076=DIRECTION('',(0.,0.,-1.));
#6077=DIRECTION('',(0.,-1.,0.));
#6078=DIRECTION('',(0.,0.,1.));
#6079=DIRECTION('',(0.,1.,0.));
#6080=DIRECTION('center_axis',(0.,0.,1.));
#6081=DIRECTION('ref_axis',(1.,0.,0.));
#6082=DIRECTION('center_axis',(0.,0.,1.));
#6083=DIRECTION('ref_axis',(1.,0.,0.));
#6084=DIRECTION('center_axis',(0.,0.,1.));
#6085=DIRECTION('ref_axis',(1.,0.,0.));
#6086=DIRECTION('center_axis',(0.,0.,1.));
#6087=DIRECTION('ref_axis',(-1.,1.22464679914735E-16,0.));
#6088=DIRECTION('center_axis',(0.,0.,1.));
#6089=DIRECTION('ref_axis',(1.,0.,0.));
#6090=DIRECTION('center_axis',(0.,0.,1.));
#6091=DIRECTION('ref_axis',(1.,0.,0.));
#6092=DIRECTION('center_axis',(0.,0.,1.));
#6093=DIRECTION('ref_axis',(1.,0.,0.));
#6094=DIRECTION('',(0.,0.,1.));
#6095=DIRECTION('center_axis',(0.,0.,1.));
#6096=DIRECTION('ref_axis',(1.,0.,0.));
#6097=DIRECTION('center_axis',(0.,0.,1.));
#6098=DIRECTION('ref_axis',(1.,0.,0.));
#6099=DIRECTION('center_axis',(0.,0.,-1.));
#6100=DIRECTION('ref_axis',(1.,0.,0.));
#6101=DIRECTION('center_axis',(0.,0.,1.));
#6102=DIRECTION('ref_axis',(1.,0.,0.));
#6103=DIRECTION('center_axis',(0.,0.,1.));
#6104=DIRECTION('ref_axis',(1.,0.,0.));
#6105=DIRECTION('center_axis',(0.,0.,1.));
#6106=DIRECTION('ref_axis',(1.,0.,0.));
#6107=DIRECTION('',(0.,0.,1.));
#6108=DIRECTION('center_axis',(0.,0.,1.));
#6109=DIRECTION('ref_axis',(1.,0.,0.));
#6110=DIRECTION('',(0.,0.,1.));
#6111=DIRECTION('center_axis',(0.,0.,-1.));
#6112=DIRECTION('ref_axis',(1.,0.,0.));
#6113=DIRECTION('center_axis',(0.,0.,1.));
#6114=DIRECTION('ref_axis',(1.,0.,0.));
#6115=DIRECTION('center_axis',(0.,0.,1.));
#6116=DIRECTION('ref_axis',(1.,0.,0.));
#6117=DIRECTION('center_axis',(0.,0.,1.));
#6118=DIRECTION('ref_axis',(1.,0.,0.));
#6119=DIRECTION('',(0.5,-0.866025403784439,0.));
#6120=DIRECTION('',(1.,-3.43386193997065E-16,0.));
#6121=DIRECTION('',(0.5,0.866025403784439,0.));
#6122=DIRECTION('',(0.,1.,0.));
#6123=DIRECTION('',(1.,0.,0.));
#6124=DIRECTION('',(0.,-1.,0.));
#6125=DIRECTION('center_axis',(0.,1.,0.));
#6126=DIRECTION('ref_axis',(-1.,0.,0.));
#6127=DIRECTION('',(-1.,0.,0.));
#6128=DIRECTION('',(0.,0.,1.));
#6129=DIRECTION('',(-1.,0.,0.));
#6130=DIRECTION('',(0.,0.,1.));
#6131=DIRECTION('center_axis',(1.,0.,0.));
#6132=DIRECTION('ref_axis',(0.,1.,0.));
#6133=DIRECTION('',(0.,-1.,0.));
#6134=DIRECTION('',(0.,1.,0.));
#6135=DIRECTION('',(0.,1.,0.));
#6136=DIRECTION('',(0.,0.,1.));
#6137=DIRECTION('center_axis',(0.,-1.,0.));
#6138=DIRECTION('ref_axis',(1.,0.,0.));
#6139=DIRECTION('',(1.,0.,0.));
#6140=DIRECTION('',(0.,0.,1.));
#6141=DIRECTION('center_axis',(-1.,0.,0.));
#6142=DIRECTION('ref_axis',(0.,-1.,0.));
#6143=DIRECTION('',(0.,-1.,0.));
#6144=DIRECTION('',(0.,1.,0.));
#6145=DIRECTION('',(0.,-1.,0.));
#6146=DIRECTION('center_axis',(0.,0.,1.));
#6147=DIRECTION('ref_axis',(1.,0.,0.));
#6148=DIRECTION('center_axis',(0.,0.,1.));
#6149=DIRECTION('ref_axis',(1.,0.,0.));
#6150=DIRECTION('',(-0.5,-0.866025403784439,0.));
#6151=DIRECTION('',(-0.5,0.866025403784439,0.));
#6152=DIRECTION('',(-1.,0.,0.));
#6153=DIRECTION('center_axis',(0.,0.,1.));
#6154=DIRECTION('ref_axis',(1.,0.,0.));
#6155=DIRECTION('',(0.5,0.866025403784439,0.));
#6156=DIRECTION('',(-0.5,0.866025403784439,0.));
#6157=DIRECTION('center_axis',(0.,0.,1.));
#6158=DIRECTION('ref_axis',(1.,0.,0.));
#6159=DIRECTION('',(0.5,0.866025403784439,0.));
#6160=DIRECTION('',(1.,-3.43386193997065E-16,0.));
#6161=DIRECTION('',(0.5,-0.866025403784439,0.));
#6162=DIRECTION('',(-0.5,-0.866025403784438,0.));
#6163=DIRECTION('',(-1.,0.,0.));
#6164=DIRECTION('',(-0.5,0.866025403784439,0.));
#6165=DIRECTION('center_axis',(0.,0.,1.));
#6166=DIRECTION('ref_axis',(1.,0.,0.));
#6167=DIRECTION('center_axis',(-3.43386193997065E-16,-1.,0.));
#6168=DIRECTION('ref_axis',(1.,-3.43386193997065E-16,0.));
#6169=DIRECTION('',(0.,0.,1.));
#6170=DIRECTION('',(0.,0.,1.));
#6171=DIRECTION('center_axis',(-0.866025403784439,-0.5,0.));
#6172=DIRECTION('ref_axis',(0.5,-0.866025403784439,0.));
#6173=DIRECTION('',(0.5,-0.866025403784439,0.));
#6174=DIRECTION('',(0.,0.,1.));
#6175=DIRECTION('center_axis',(-0.866025403784439,0.5,0.));
#6176=DIRECTION('ref_axis',(-0.5,-0.866025403784439,0.));
#6177=DIRECTION('',(-0.5,-0.866025403784438,0.));
#6178=DIRECTION('',(0.,0.,1.));
#6179=DIRECTION('center_axis',(0.,1.,0.));
#6180=DIRECTION('ref_axis',(-1.,0.,0.));
#6181=DIRECTION('',(0.,0.,1.));
#6182=DIRECTION('center_axis',(0.866025403784439,0.5,0.));
#6183=DIRECTION('ref_axis',(-0.5,0.866025403784439,0.));
#6184=DIRECTION('',(0.,0.,1.));
#6185=DIRECTION('center_axis',(0.866025403784439,-0.5,0.));
#6186=DIRECTION('ref_axis',(0.5,0.866025403784439,0.));
#6187=DIRECTION('center_axis',(0.,0.,1.));
#6188=DIRECTION('ref_axis',(1.,0.,0.));
#6189=DIRECTION('center_axis',(0.,0.,1.));
#6190=DIRECTION('ref_axis',(1.,0.,0.));
#6191=DIRECTION('',(0.,0.,-1.));
#6192=DIRECTION('center_axis',(0.,0.,-1.));
#6193=DIRECTION('ref_axis',(1.,0.,0.));
#6194=DIRECTION('center_axis',(0.,0.,1.));
#6195=DIRECTION('ref_axis',(1.,0.,0.));
#6196=DIRECTION('',(0.,0.,-1.));
#6197=DIRECTION('center_axis',(0.,0.,1.));
#6198=DIRECTION('ref_axis',(1.,0.,0.));
#6199=DIRECTION('center_axis',(0.,0.,1.));
#6200=DIRECTION('ref_axis',(1.,0.,0.));
#6201=DIRECTION('axis',(0.,0.,1.));
#6202=DIRECTION('refdir',(1.,0.,0.));
#6203=DIRECTION('center_axis',(0.,0.,1.));
#6204=DIRECTION('ref_axis',(1.,0.,0.));
#6205=DIRECTION('center_axis',(0.,0.,1.));
#6206=DIRECTION('ref_axis',(1.,0.,0.));
#6207=DIRECTION('',(0.707106781186549,8.65956056235495E-17,-0.707106781186546));
#6208=DIRECTION('center_axis',(0.,0.,1.));
#6209=DIRECTION('ref_axis',(1.,0.,0.));
#6210=DIRECTION('center_axis',(0.,0.,1.));
#6211=DIRECTION('ref_axis',(1.,0.,0.));
#6212=DIRECTION('',(0.316227766016837,3.87267321454038E-17,-0.948683298050514));
#6213=DIRECTION('center_axis',(0.,0.,1.));
#6214=DIRECTION('ref_axis',(1.,0.,0.));
#6215=DIRECTION('center_axis',(0.,0.,1.));
#6216=DIRECTION('ref_axis',(1.,0.,0.));
#6217=DIRECTION('',(0.,0.,-1.));
#6218=DIRECTION('center_axis',(0.,0.,-1.));
#6219=DIRECTION('ref_axis',(-1.,0.,0.));
#6220=DIRECTION('center_axis',(0.,0.,1.));
#6221=DIRECTION('ref_axis',(1.,0.,0.));
#6222=DIRECTION('center_axis',(0.,0.,1.));
#6223=DIRECTION('ref_axis',(1.,0.,0.));
#6224=DIRECTION('center_axis',(0.,0.,1.));
#6225=DIRECTION('ref_axis',(1.,0.,0.));
#6226=DIRECTION('',(0.,0.,-1.));
#6227=DIRECTION('center_axis',(0.,0.,1.));
#6228=DIRECTION('ref_axis',(1.,0.,0.));
#6229=DIRECTION('axis',(0.,0.,1.));
#6230=DIRECTION('refdir',(1.,0.,0.));
#6231=DIRECTION('center_axis',(0.,0.,1.));
#6232=DIRECTION('ref_axis',(1.,0.,0.));
#6233=DIRECTION('center_axis',(0.,0.,1.));
#6234=DIRECTION('ref_axis',(1.,0.,0.));
#6235=DIRECTION('',(0.,0.,1.));
#6236=DIRECTION('center_axis',(0.,0.,1.));
#6237=DIRECTION('ref_axis',(1.,0.,0.));
#6238=DIRECTION('center_axis',(0.,0.,1.));
#6239=DIRECTION('ref_axis',(1.,0.,0.));
#6240=DIRECTION('center_axis',(0.,0.,1.));
#6241=DIRECTION('ref_axis',(1.,0.,0.));
#6242=DIRECTION('center_axis',(0.,0.,1.));
#6243=DIRECTION('ref_axis',(1.,0.,0.));
#6244=DIRECTION('',(0.,0.,1.));
#6245=DIRECTION('center_axis',(0.,0.,1.));
#6246=DIRECTION('ref_axis',(1.,0.,0.));
#6247=DIRECTION('center_axis',(0.,0.,1.));
#6248=DIRECTION('ref_axis',(1.,0.,0.));
#6249=DIRECTION('center_axis',(0.,1.,0.));
#6250=DIRECTION('ref_axis',(1.,0.,0.));
#6251=DIRECTION('',(1.,0.,0.));
#6252=DIRECTION('center_axis',(0.,1.,0.));
#6253=DIRECTION('ref_axis',(1.,0.,0.));
#6254=DIRECTION('center_axis',(0.,1.,0.));
#6255=DIRECTION('ref_axis',(1.,0.,0.));
#6256=DIRECTION('',(0.,0.,1.));
#6257=DIRECTION('center_axis',(0.,1.,0.));
#6258=DIRECTION('ref_axis',(1.,0.,0.));
#6259=DIRECTION('center_axis',(0.,1.,0.));
#6260=DIRECTION('ref_axis',(1.,0.,0.));
#6261=DIRECTION('',(0.,0.,-1.));
#6262=DIRECTION('center_axis',(0.,1.,0.));
#6263=DIRECTION('ref_axis',(1.,0.,0.));
#6264=DIRECTION('center_axis',(0.,1.,0.));
#6265=DIRECTION('ref_axis',(1.,0.,0.));
#6266=DIRECTION('',(0.,1.,0.));
#6267=DIRECTION('center_axis',(0.,1.,0.));
#6268=DIRECTION('ref_axis',(1.,0.,0.));
#6269=DIRECTION('',(0.,-1.,0.));
#6270=DIRECTION('center_axis',(0.,1.,0.));
#6271=DIRECTION('ref_axis',(1.,0.,0.));
#6272=DIRECTION('',(0.,1.,0.));
#6273=DIRECTION('center_axis',(0.,-0.707106781186549,-0.707106781186546));
#6274=DIRECTION('ref_axis',(0.,0.707106781186546,-0.707106781186549));
#6275=DIRECTION('center_axis',(0.,-0.707106781186549,0.707106781186546));
#6276=DIRECTION('ref_axis',(0.,-0.707106781186546,-0.707106781186549));
#6277=DIRECTION('',(0.,-1.,0.));
#6278=DIRECTION('',(0.,1.,0.));
#6279=DIRECTION('center_axis',(0.,-0.707106781186549,0.707106781186546));
#6280=DIRECTION('ref_axis',(0.,-0.707106781186546,-0.707106781186549));
#6281=DIRECTION('center_axis',(0.,1.,0.));
#6282=DIRECTION('ref_axis',(1.,0.,0.));
#6283=DIRECTION('center_axis',(0.,1.,0.));
#6284=DIRECTION('ref_axis',(1.,0.,0.));
#6285=DIRECTION('center_axis',(0.,0.707106781186549,-0.707106781186546));
#6286=DIRECTION('ref_axis',(0.,-0.707106781186546,-0.707106781186549));
#6287=DIRECTION('center_axis',(0.,0.707106781186549,0.707106781186546));
#6288=DIRECTION('ref_axis',(0.,0.707106781186546,-0.707106781186549));
#6289=DIRECTION('center_axis',(0.,1.,0.));
#6290=DIRECTION('ref_axis',(-1.,0.,1.22464679914735E-16));
#6291=DIRECTION('center_axis',(0.,0.707106781186549,-0.707106781186546));
#6292=DIRECTION('ref_axis',(0.,-0.707106781186546,-0.707106781186549));
#6293=DIRECTION('center_axis',(0.,0.707106781186549,0.707106781186546));
#6294=DIRECTION('ref_axis',(0.,0.707106781186546,-0.707106781186549));
#6295=DIRECTION('center_axis',(0.,1.,0.));
#6296=DIRECTION('ref_axis',(1.,0.,0.));
#6297=DIRECTION('center_axis',(0.,1.,0.));
#6298=DIRECTION('ref_axis',(1.,0.,0.));
#6299=DIRECTION('center_axis',(0.,0.,1.));
#6300=DIRECTION('ref_axis',(1.,0.,0.));
#6301=DIRECTION('center_axis',(0.,0.,1.));
#6302=DIRECTION('ref_axis',(1.,0.,0.));
#6303=DIRECTION('center_axis',(0.,0.,1.));
#6304=DIRECTION('ref_axis',(1.,0.,0.));
#6305=DIRECTION('center_axis',(0.,0.,1.));
#6306=DIRECTION('ref_axis',(1.,0.,0.));
#6307=DIRECTION('center_axis',(0.,0.,1.));
#6308=DIRECTION('ref_axis',(1.,0.,0.));
#6309=DIRECTION('center_axis',(0.,0.,1.));
#6310=DIRECTION('ref_axis',(1.,0.,0.));
#6311=DIRECTION('center_axis',(0.,0.,1.));
#6312=DIRECTION('ref_axis',(1.,0.,0.));
#6313=DIRECTION('center_axis',(0.,0.,1.));
#6314=DIRECTION('ref_axis',(-1.,5.20660583828602E-15,0.));
#6315=DIRECTION('center_axis',(0.,0.,1.));
#6316=DIRECTION('ref_axis',(1.,0.,0.));
#6317=DIRECTION('',(0.,0.,1.));
#6318=DIRECTION('center_axis',(0.,0.,-1.));
#6319=DIRECTION('ref_axis',(1.,0.,0.));
#6320=DIRECTION('center_axis',(0.,1.,0.));
#6321=DIRECTION('ref_axis',(1.,0.,0.));
#6322=DIRECTION('center_axis',(0.,1.,0.));
#6323=DIRECTION('ref_axis',(1.,0.,0.));
#6324=DIRECTION('center_axis',(0.,1.,0.));
#6325=DIRECTION('ref_axis',(1.,0.,0.));
#6326=DIRECTION('center_axis',(0.,0.,1.));
#6327=DIRECTION('ref_axis',(1.,0.,0.));
#6328=DIRECTION('center_axis',(0.,0.,1.));
#6329=DIRECTION('ref_axis',(1.,0.,0.));
#6330=DIRECTION('',(0.,0.,1.));
#6331=DIRECTION('center_axis',(0.,0.,-1.));
#6332=DIRECTION('ref_axis',(1.,0.,0.));
#6333=DIRECTION('center_axis',(0.,0.,1.));
#6334=DIRECTION('ref_axis',(1.,0.,0.));
#6335=DIRECTION('center_axis',(0.,1.,0.));
#6336=DIRECTION('ref_axis',(1.,0.,0.));
#6337=DIRECTION('center_axis',(0.,1.,0.));
#6338=DIRECTION('ref_axis',(1.,0.,0.));
#6339=DIRECTION('',(0.,1.,0.));
#6340=DIRECTION('center_axis',(0.,-1.,0.));
#6341=DIRECTION('ref_axis',(1.,0.,0.));
#6342=DIRECTION('center_axis',(0.,1.,0.));
#6343=DIRECTION('ref_axis',(1.,0.,0.));
#6344=DIRECTION('center_axis',(0.,1.,0.));
#6345=DIRECTION('ref_axis',(1.,0.,0.));
#6346=DIRECTION('',(0.,1.,0.));
#6347=DIRECTION('center_axis',(0.,-1.,0.));
#6348=DIRECTION('ref_axis',(1.,0.,0.));
#6349=DIRECTION('center_axis',(0.,1.,0.));
#6350=DIRECTION('ref_axis',(1.,0.,0.));
#6351=DIRECTION('center_axis',(0.,1.,0.));
#6352=DIRECTION('ref_axis',(1.,0.,0.));
#6353=DIRECTION('',(0.,1.,0.));
#6354=DIRECTION('center_axis',(0.,-1.,0.));
#6355=DIRECTION('ref_axis',(1.,0.,0.));
#6356=DIRECTION('center_axis',(0.,1.,0.));
#6357=DIRECTION('ref_axis',(1.,0.,0.));
#6358=DIRECTION('center_axis',(0.,1.,0.));
#6359=DIRECTION('ref_axis',(1.,0.,0.));
#6360=DIRECTION('',(0.,1.,0.));
#6361=DIRECTION('center_axis',(0.,-1.,0.));
#6362=DIRECTION('ref_axis',(1.,0.,0.));
#6363=DIRECTION('center_axis',(0.,1.,0.));
#6364=DIRECTION('ref_axis',(1.,0.,0.));
#6365=DIRECTION('center_axis',(0.,1.,0.));
#6366=DIRECTION('ref_axis',(1.,0.,0.));
#6367=DIRECTION('',(0.,1.,0.));
#6368=DIRECTION('center_axis',(0.,1.,0.));
#6369=DIRECTION('ref_axis',(-1.,0.,0.));
#6370=DIRECTION('',(-1.,0.,0.));
#6371=DIRECTION('',(0.,0.,1.));
#6372=DIRECTION('',(-1.,0.,0.));
#6373=DIRECTION('',(0.,0.,1.));
#6374=DIRECTION('center_axis',(1.,0.,0.));
#6375=DIRECTION('ref_axis',(0.,1.,0.));
#6376=DIRECTION('',(0.,1.,0.));
#6377=DIRECTION('',(0.,1.,0.));
#6378=DIRECTION('',(0.,0.,1.));
#6379=DIRECTION('center_axis',(0.,-1.,0.));
#6380=DIRECTION('ref_axis',(1.,0.,0.));
#6381=DIRECTION('',(1.,0.,0.));
#6382=DIRECTION('',(1.,0.,0.));
#6383=DIRECTION('',(0.,0.,1.));
#6384=DIRECTION('center_axis',(-1.,0.,0.));
#6385=DIRECTION('ref_axis',(0.,-1.,0.));
#6386=DIRECTION('',(0.,-1.,0.));
#6387=DIRECTION('',(0.,-1.,0.));
#6388=DIRECTION('center_axis',(0.,0.,1.));
#6389=DIRECTION('ref_axis',(1.,0.,0.));
#6390=DIRECTION('center_axis',(0.,0.,1.));
#6391=DIRECTION('ref_axis',(1.,0.,0.));
#6392=DIRECTION('axis',(0.,0.,1.));
#6393=DIRECTION('refdir',(1.,0.,0.));
#6394=DIRECTION('center_axis',(1.,0.,0.));
#6395=DIRECTION('ref_axis',(0.,0.,-1.));
#6396=DIRECTION('center_axis',(1.,0.,0.));
#6397=DIRECTION('ref_axis',(0.,0.,-1.));
#6398=DIRECTION('',(1.,0.,0.));
#6399=DIRECTION('center_axis',(-1.,0.,0.));
#6400=DIRECTION('ref_axis',(0.,0.,-1.));
#6401=DIRECTION('center_axis',(1.,0.,0.));
#6402=DIRECTION('ref_axis',(0.,0.,-1.));
#6403=DIRECTION('',(0.,0.,-1.));
#6404=DIRECTION('',(0.,-1.,0.));
#6405=DIRECTION('',(0.,0.,1.));
#6406=DIRECTION('',(0.,1.,0.));
#6407=DIRECTION('center_axis',(0.,0.,1.));
#6408=DIRECTION('ref_axis',(1.,0.,0.));
#6409=DIRECTION('center_axis',(0.,0.,1.));
#6410=DIRECTION('ref_axis',(1.,0.,0.));
#6411=DIRECTION('center_axis',(0.,0.,1.));
#6412=DIRECTION('ref_axis',(1.,0.,0.));
#6413=DIRECTION('center_axis',(0.,0.,1.));
#6414=DIRECTION('ref_axis',(-1.,1.22464679914735E-16,0.));
#6415=DIRECTION('center_axis',(0.,0.,1.));
#6416=DIRECTION('ref_axis',(1.,0.,0.));
#6417=DIRECTION('center_axis',(0.,0.,1.));
#6418=DIRECTION('ref_axis',(1.,0.,0.));
#6419=DIRECTION('center_axis',(0.,0.,1.));
#6420=DIRECTION('ref_axis',(1.,0.,0.));
#6421=DIRECTION('',(0.,0.,1.));
#6422=DIRECTION('center_axis',(0.,0.,1.));
#6423=DIRECTION('ref_axis',(1.,0.,0.));
#6424=DIRECTION('center_axis',(0.,0.,1.));
#6425=DIRECTION('ref_axis',(1.,0.,0.));
#6426=DIRECTION('center_axis',(0.,0.,-1.));
#6427=DIRECTION('ref_axis',(1.,0.,0.));
#6428=DIRECTION('center_axis',(0.,0.,1.));
#6429=DIRECTION('ref_axis',(1.,0.,0.));
#6430=DIRECTION('center_axis',(0.,0.,1.));
#6431=DIRECTION('ref_axis',(1.,0.,0.));
#6432=DIRECTION('center_axis',(0.,0.,1.));
#6433=DIRECTION('ref_axis',(1.,0.,0.));
#6434=DIRECTION('',(0.,0.,1.));
#6435=DIRECTION('center_axis',(0.,0.,1.));
#6436=DIRECTION('ref_axis',(1.,0.,0.));
#6437=DIRECTION('',(0.,0.,1.));
#6438=DIRECTION('center_axis',(0.,0.,-1.));
#6439=DIRECTION('ref_axis',(1.,0.,0.));
#6440=DIRECTION('center_axis',(0.,0.,1.));
#6441=DIRECTION('ref_axis',(1.,0.,0.));
#6442=DIRECTION('center_axis',(0.,0.,1.));
#6443=DIRECTION('ref_axis',(1.,0.,0.));
#6444=DIRECTION('center_axis',(0.,0.,1.));
#6445=DIRECTION('ref_axis',(1.,0.,0.));
#6446=DIRECTION('',(0.5,-0.866025403784439,0.));
#6447=DIRECTION('',(1.,0.,0.));
#6448=DIRECTION('',(0.5,0.866025403784439,0.));
#6449=DIRECTION('',(0.,1.,0.));
#6450=DIRECTION('',(1.,0.,0.));
#6451=DIRECTION('',(0.,-1.,0.));
#6452=DIRECTION('center_axis',(0.,1.,0.));
#6453=DIRECTION('ref_axis',(-1.,0.,0.));
#6454=DIRECTION('',(-1.,0.,0.));
#6455=DIRECTION('',(0.,0.,1.));
#6456=DIRECTION('',(-1.,0.,0.));
#6457=DIRECTION('',(0.,0.,1.));
#6458=DIRECTION('center_axis',(1.,0.,0.));
#6459=DIRECTION('ref_axis',(0.,1.,0.));
#6460=DIRECTION('',(0.,-1.,0.));
#6461=DIRECTION('',(0.,1.,0.));
#6462=DIRECTION('',(0.,1.,0.));
#6463=DIRECTION('',(0.,0.,1.));
#6464=DIRECTION('center_axis',(0.,-1.,0.));
#6465=DIRECTION('ref_axis',(1.,0.,0.));
#6466=DIRECTION('',(1.,0.,0.));
#6467=DIRECTION('',(0.,0.,1.));
#6468=DIRECTION('center_axis',(-1.,0.,0.));
#6469=DIRECTION('ref_axis',(0.,-1.,0.));
#6470=DIRECTION('',(0.,-1.,0.));
#6471=DIRECTION('',(0.,1.,0.));
#6472=DIRECTION('',(0.,-1.,0.));
#6473=DIRECTION('center_axis',(0.,0.,1.));
#6474=DIRECTION('ref_axis',(1.,0.,0.));
#6475=DIRECTION('center_axis',(0.,0.,1.));
#6476=DIRECTION('ref_axis',(1.,0.,0.));
#6477=DIRECTION('',(-0.5,-0.866025403784439,0.));
#6478=DIRECTION('',(-0.5,0.866025403784439,0.));
#6479=DIRECTION('',(-1.,0.,0.));
#6480=DIRECTION('center_axis',(0.,0.,1.));
#6481=DIRECTION('ref_axis',(1.,0.,0.));
#6482=DIRECTION('',(0.5,0.866025403784439,0.));
#6483=DIRECTION('',(-0.5,0.866025403784439,0.));
#6484=DIRECTION('center_axis',(0.,0.,1.));
#6485=DIRECTION('ref_axis',(1.,0.,0.));
#6486=DIRECTION('',(0.5,0.866025403784439,0.));
#6487=DIRECTION('',(1.,0.,0.));
#6488=DIRECTION('',(0.5,-0.866025403784439,0.));
#6489=DIRECTION('',(-0.5,-0.866025403784439,0.));
#6490=DIRECTION('',(-1.,0.,0.));
#6491=DIRECTION('',(-0.5,0.866025403784439,0.));
#6492=DIRECTION('center_axis',(0.,0.,1.));
#6493=DIRECTION('ref_axis',(1.,0.,0.));
#6494=DIRECTION('center_axis',(0.,-1.,0.));
#6495=DIRECTION('ref_axis',(1.,0.,0.));
#6496=DIRECTION('',(0.,0.,1.));
#6497=DIRECTION('',(0.,0.,1.));
#6498=DIRECTION('center_axis',(-0.866025403784439,-0.5,0.));
#6499=DIRECTION('ref_axis',(0.5,-0.866025403784439,0.));
#6500=DIRECTION('',(0.5,-0.866025403784439,0.));
#6501=DIRECTION('',(0.,0.,1.));
#6502=DIRECTION('center_axis',(-0.866025403784439,0.5,0.));
#6503=DIRECTION('ref_axis',(-0.5,-0.866025403784439,0.));
#6504=DIRECTION('',(-0.5,-0.866025403784439,0.));
#6505=DIRECTION('',(0.,0.,1.));
#6506=DIRECTION('center_axis',(0.,1.,0.));
#6507=DIRECTION('ref_axis',(-1.,0.,0.));
#6508=DIRECTION('',(0.,0.,1.));
#6509=DIRECTION('center_axis',(0.866025403784439,0.5,0.));
#6510=DIRECTION('ref_axis',(-0.5,0.866025403784439,0.));
#6511=DIRECTION('',(0.,0.,1.));
#6512=DIRECTION('center_axis',(0.866025403784439,-0.5,0.));
#6513=DIRECTION('ref_axis',(0.5,0.866025403784439,0.));
#6514=DIRECTION('center_axis',(0.,0.,1.));
#6515=DIRECTION('ref_axis',(1.,0.,0.));
#6516=DIRECTION('center_axis',(0.,0.,1.));
#6517=DIRECTION('ref_axis',(1.,0.,0.));
#6518=DIRECTION('',(0.,0.,-1.));
#6519=DIRECTION('center_axis',(0.,0.,-1.));
#6520=DIRECTION('ref_axis',(1.,0.,0.));
#6521=DIRECTION('center_axis',(0.,0.,1.));
#6522=DIRECTION('ref_axis',(1.,0.,0.));
#6523=DIRECTION('',(0.,0.,-1.));
#6524=DIRECTION('center_axis',(0.,0.,1.));
#6525=DIRECTION('ref_axis',(1.,0.,0.));
#6526=DIRECTION('center_axis',(0.,0.,1.));
#6527=DIRECTION('ref_axis',(1.,0.,0.));
#6528=DIRECTION('axis',(0.,0.,1.));
#6529=DIRECTION('refdir',(1.,0.,0.));
#6530=DIRECTION('center_axis',(0.,0.,1.));
#6531=DIRECTION('ref_axis',(1.,0.,0.));
#6532=DIRECTION('center_axis',(0.,0.,1.));
#6533=DIRECTION('ref_axis',(1.,0.,0.));
#6534=DIRECTION('',(0.707106781186549,8.65956056235495E-17,-0.707106781186546));
#6535=DIRECTION('center_axis',(0.,0.,1.));
#6536=DIRECTION('ref_axis',(1.,0.,0.));
#6537=DIRECTION('center_axis',(0.,0.,1.));
#6538=DIRECTION('ref_axis',(1.,0.,0.));
#6539=DIRECTION('',(0.316227766016837,3.87267321454038E-17,-0.948683298050514));
#6540=DIRECTION('center_axis',(0.,0.,1.));
#6541=DIRECTION('ref_axis',(1.,0.,0.));
#6542=DIRECTION('center_axis',(0.,0.,1.));
#6543=DIRECTION('ref_axis',(1.,0.,0.));
#6544=DIRECTION('',(0.,0.,-1.));
#6545=DIRECTION('center_axis',(0.,0.,-1.));
#6546=DIRECTION('ref_axis',(-1.,0.,0.));
#6547=DIRECTION('center_axis',(0.,0.,1.));
#6548=DIRECTION('ref_axis',(1.,0.,0.));
#6549=DIRECTION('center_axis',(0.,0.,1.));
#6550=DIRECTION('ref_axis',(1.,0.,0.));
#6551=DIRECTION('center_axis',(0.,0.,1.));
#6552=DIRECTION('ref_axis',(1.,0.,0.));
#6553=DIRECTION('',(0.,0.,-1.));
#6554=DIRECTION('center_axis',(0.,0.,1.));
#6555=DIRECTION('ref_axis',(1.,0.,0.));
#6556=DIRECTION('axis',(0.,0.,1.));
#6557=DIRECTION('refdir',(1.,0.,0.));
#6558=DIRECTION('center_axis',(0.,1.,0.));
#6559=DIRECTION('ref_axis',(1.,0.,0.));
#6560=DIRECTION('center_axis',(0.,-1.,0.));
#6561=DIRECTION('ref_axis',(1.,0.,0.));
#6562=DIRECTION('',(0.,-1.,0.));
#6563=DIRECTION('center_axis',(0.,-1.,0.));
#6564=DIRECTION('ref_axis',(1.,0.,0.));
#6565=DIRECTION('center_axis',(0.,1.,0.));
#6566=DIRECTION('ref_axis',(1.,0.,0.));
#6567=DIRECTION('center_axis',(0.,1.,0.));
#6568=DIRECTION('ref_axis',(1.,0.,0.));
#6569=DIRECTION('',(0.,-1.,0.));
#6570=DIRECTION('center_axis',(0.,1.,0.));
#6571=DIRECTION('ref_axis',(1.,0.,0.));
#6572=DIRECTION('center_axis',(0.,1.,0.));
#6573=DIRECTION('ref_axis',(1.,0.,0.));
#6574=DIRECTION('center_axis',(0.,1.,0.));
#6575=DIRECTION('ref_axis',(1.,0.,0.));
#6576=DIRECTION('axis',(0.,0.,1.));
#6577=DIRECTION('refdir',(1.,0.,0.));
#6578=DIRECTION('center_axis',(0.,1.,0.));
#6579=DIRECTION('ref_axis',(1.,0.,0.));
#6580=DIRECTION('center_axis',(0.,-1.,0.));
#6581=DIRECTION('ref_axis',(1.,0.,0.));
#6582=DIRECTION('',(0.,-1.,0.));
#6583=DIRECTION('center_axis',(0.,-1.,0.));
#6584=DIRECTION('ref_axis',(1.,0.,0.));
#6585=DIRECTION('center_axis',(0.,1.,0.));
#6586=DIRECTION('ref_axis',(1.,0.,0.));
#6587=DIRECTION('center_axis',(0.,1.,0.));
#6588=DIRECTION('ref_axis',(1.,0.,0.));
#6589=DIRECTION('',(0.,-1.,0.));
#6590=DIRECTION('center_axis',(0.,1.,0.));
#6591=DIRECTION('ref_axis',(1.,0.,0.));
#6592=DIRECTION('center_axis',(0.,1.,0.));
#6593=DIRECTION('ref_axis',(1.,0.,0.));
#6594=DIRECTION('center_axis',(0.,1.,0.));
#6595=DIRECTION('ref_axis',(1.,0.,0.));
#6596=DIRECTION('axis',(0.,0.,1.));
#6597=DIRECTION('refdir',(1.,0.,0.));
#6598=DIRECTION('center_axis',(0.,1.,0.));
#6599=DIRECTION('ref_axis',(1.,0.,0.));
#6600=DIRECTION('center_axis',(0.,-1.,0.));
#6601=DIRECTION('ref_axis',(1.,0.,0.));
#6602=DIRECTION('',(0.,-1.,0.));
#6603=DIRECTION('center_axis',(0.,-1.,0.));
#6604=DIRECTION('ref_axis',(1.,0.,0.));
#6605=DIRECTION('center_axis',(0.,1.,0.));
#6606=DIRECTION('ref_axis',(1.,0.,0.));
#6607=DIRECTION('center_axis',(0.,1.,0.));
#6608=DIRECTION('ref_axis',(1.,0.,0.));
#6609=DIRECTION('',(0.,-1.,0.));
#6610=DIRECTION('center_axis',(0.,1.,0.));
#6611=DIRECTION('ref_axis',(1.,0.,0.));
#6612=DIRECTION('center_axis',(0.,1.,0.));
#6613=DIRECTION('ref_axis',(1.,0.,0.));
#6614=DIRECTION('center_axis',(0.,1.,0.));
#6615=DIRECTION('ref_axis',(1.,0.,0.));
#6616=DIRECTION('axis',(0.,0.,1.));
#6617=DIRECTION('refdir',(1.,0.,0.));
#6618=DIRECTION('center_axis',(0.,0.,1.));
#6619=DIRECTION('ref_axis',(1.,0.,0.));
#6620=DIRECTION('center_axis',(0.,0.,1.));
#6621=DIRECTION('ref_axis',(1.,0.,0.));
#6622=DIRECTION('',(0.,0.,1.));
#6623=DIRECTION('center_axis',(0.,0.,-1.));
#6624=DIRECTION('ref_axis',(1.,0.,0.));
#6625=DIRECTION('center_axis',(0.,0.,1.));
#6626=DIRECTION('ref_axis',(1.,0.,0.));
#6627=DIRECTION('center_axis',(0.,0.,1.));
#6628=DIRECTION('ref_axis',(1.,0.,0.));
#6629=DIRECTION('',(0.,0.,1.));
#6630=DIRECTION('center_axis',(0.,0.,-1.));
#6631=DIRECTION('ref_axis',(1.,0.,0.));
#6632=DIRECTION('center_axis',(0.,0.,1.));
#6633=DIRECTION('ref_axis',(1.,0.,0.));
#6634=DIRECTION('center_axis',(0.,0.,1.));
#6635=DIRECTION('ref_axis',(1.,0.,0.));
#6636=DIRECTION('',(0.,0.,1.));
#6637=DIRECTION('center_axis',(0.,0.,1.));
#6638=DIRECTION('ref_axis',(1.,0.,0.));
#6639=DIRECTION('center_axis',(0.,0.,1.));
#6640=DIRECTION('ref_axis',(1.,0.,0.));
#6641=DIRECTION('center_axis',(0.,0.,-1.));
#6642=DIRECTION('ref_axis',(1.,0.,0.));
#6643=DIRECTION('center_axis',(0.,0.,1.));
#6644=DIRECTION('ref_axis',(1.,0.,0.));
#6645=DIRECTION('center_axis',(0.,0.,1.));
#6646=DIRECTION('ref_axis',(1.,0.,0.));
#6647=DIRECTION('',(0.,0.,1.));
#6648=DIRECTION('center_axis',(0.,0.,1.));
#6649=DIRECTION('ref_axis',(1.,0.,0.));
#6650=DIRECTION('center_axis',(0.,0.,1.));
#6651=DIRECTION('ref_axis',(1.,0.,0.));
#6652=DIRECTION('center_axis',(0.,0.,-1.));
#6653=DIRECTION('ref_axis',(1.,0.,0.));
#6654=DIRECTION('center_axis',(0.,0.,1.));
#6655=DIRECTION('ref_axis',(1.,0.,0.));
#6656=DIRECTION('',(0.,0.,1.));
#6657=DIRECTION('center_axis',(0.,0.,-1.));
#6658=DIRECTION('ref_axis',(1.,0.,0.));
#6659=DIRECTION('center_axis',(0.,0.,1.));
#6660=DIRECTION('ref_axis',(1.,0.,0.));
#6661=DIRECTION('',(0.,0.,1.));
#6662=DIRECTION('center_axis',(0.,0.,-1.));
#6663=DIRECTION('ref_axis',(1.,0.,0.));
#6664=DIRECTION('center_axis',(0.,1.,0.));
#6665=DIRECTION('ref_axis',(-1.,0.,0.));
#6666=DIRECTION('',(-1.,0.,0.));
#6667=DIRECTION('',(0.,0.,1.));
#6668=DIRECTION('',(-1.,0.,0.));
#6669=DIRECTION('',(0.,0.,1.));
#6670=DIRECTION('center_axis',(1.,0.,0.));
#6671=DIRECTION('ref_axis',(0.,1.,0.));
#6672=DIRECTION('',(0.,1.,0.));
#6673=DIRECTION('',(0.,1.,0.));
#6674=DIRECTION('',(0.,0.,1.));
#6675=DIRECTION('center_axis',(0.,-1.,0.));
#6676=DIRECTION('ref_axis',(1.,0.,0.));
#6677=DIRECTION('',(1.,0.,0.));
#6678=DIRECTION('',(1.,0.,0.));
#6679=DIRECTION('',(0.,0.,1.));
#6680=DIRECTION('center_axis',(-1.,0.,0.));
#6681=DIRECTION('ref_axis',(0.,-1.,0.));
#6682=DIRECTION('',(0.,-1.,0.));
#6683=DIRECTION('',(0.,-1.,0.));
#6684=DIRECTION('center_axis',(0.,0.,1.));
#6685=DIRECTION('ref_axis',(1.,0.,0.));
#6686=DIRECTION('center_axis',(0.,0.,1.));
#6687=DIRECTION('ref_axis',(1.,0.,0.));
#6688=DIRECTION('axis',(0.,0.,1.));
#6689=DIRECTION('refdir',(1.,0.,0.));
#6690=DIRECTION('center_axis',(0.,1.,0.));
#6691=DIRECTION('ref_axis',(0.,0.,1.));
#6692=DIRECTION('center_axis',(0.,-1.,0.));
#6693=DIRECTION('ref_axis',(1.,0.,0.));
#6694=DIRECTION('center_axis',(0.,-1.,0.));
#6695=DIRECTION('ref_axis',(1.,0.,0.));
#6696=DIRECTION('center_axis',(0.,-1.,0.));
#6697=DIRECTION('ref_axis',(1.,0.,0.));
#6698=DIRECTION('',(0.707106781186548,0.707106781186547,8.65956056235493E-17));
#6699=DIRECTION('center_axis',(0.,-1.,0.));
#6700=DIRECTION('ref_axis',(1.,0.,0.));
#6701=DIRECTION('center_axis',(0.,-1.,0.));
#6702=DIRECTION('ref_axis',(1.,0.,0.));
#6703=DIRECTION('',(0.,1.,0.));
#6704=DIRECTION('center_axis',(0.,1.,0.));
#6705=DIRECTION('ref_axis',(1.,0.,0.));
#6706=DIRECTION('center_axis',(0.,-1.,0.));
#6707=DIRECTION('ref_axis',(1.,0.,0.));
#6708=DIRECTION('',(-0.707106781186547,0.707106781186548,-8.65956056235493E-17));
#6709=DIRECTION('center_axis',(0.,-1.,0.));
#6710=DIRECTION('ref_axis',(0.,0.,-1.));
#6711=DIRECTION('center_axis',(0.,-1.,0.));
#6712=DIRECTION('ref_axis',(1.,0.,0.));
#6713=DIRECTION('center_axis',(0.,1.,0.));
#6714=DIRECTION('ref_axis',(1.,0.,0.));
#6715=DIRECTION('center_axis',(0.,1.,0.));
#6716=DIRECTION('ref_axis',(1.,0.,0.));
#6717=DIRECTION('',(-0.447213595499958,0.894427190999916,-5.47678698264203E-17));
#6718=DIRECTION('center_axis',(0.,-1.,0.));
#6719=DIRECTION('ref_axis',(1.,0.,0.));
#6720=DIRECTION('center_axis',(0.,1.,0.));
#6721=DIRECTION('ref_axis',(1.,0.,0.));
#6722=DIRECTION('',(0.,1.,0.));
#6723=DIRECTION('center_axis',(0.,1.,0.));
#6724=DIRECTION('ref_axis',(1.,0.,0.));
#6725=DIRECTION('center_axis',(0.,-1.,0.));
#6726=DIRECTION('ref_axis',(1.,0.,0.));
#6727=DIRECTION('',(-0.707106781186547,0.707106781186548,-8.65956056235493E-17));
#6728=DIRECTION('center_axis',(0.,-1.,0.));
#6729=DIRECTION('ref_axis',(0.,0.,-1.));
#6730=DIRECTION('center_axis',(0.866025403784439,0.,-0.5));
#6731=DIRECTION('ref_axis',(0.5,0.,0.866025403784439));
#6732=DIRECTION('',(-0.5,0.,-0.866025403784439));
#6733=DIRECTION('',(0.,-1.,0.));
#6734=DIRECTION('',(0.5,0.,0.866025403784439));
#6735=DIRECTION('',(0.,-1.,0.));
#6736=DIRECTION('center_axis',(1.20185167898973E-16,0.,-1.));
#6737=DIRECTION('ref_axis',(1.,0.,1.20185167898973E-16));
#6738=DIRECTION('',(-1.,0.,-1.20185167898973E-16));
#6739=DIRECTION('',(0.,-1.,0.));
#6740=DIRECTION('',(1.,0.,1.20185167898973E-16));
#6741=DIRECTION('center_axis',(-0.866025403784439,0.,-0.5));
#6742=DIRECTION('ref_axis',(0.5,0.,-0.866025403784439));
#6743=DIRECTION('',(-0.5,0.,0.866025403784439));
#6744=DIRECTION('',(0.,-1.,0.));
#6745=DIRECTION('',(0.5,0.,-0.866025403784439));
#6746=DIRECTION('center_axis',(-0.866025403784439,0.,0.5));
#6747=DIRECTION('ref_axis',(-0.5,0.,-0.866025403784439));
#6748=DIRECTION('',(0.5,0.,0.866025403784439));
#6749=DIRECTION('',(0.,-1.,0.));
#6750=DIRECTION('',(-0.5,0.,-0.866025403784439));
#6751=DIRECTION('center_axis',(-2.40370335797945E-16,0.,1.));
#6752=DIRECTION('ref_axis',(-1.,0.,-2.40370335797945E-16));
#6753=DIRECTION('',(1.,0.,2.40370335797945E-16));
#6754=DIRECTION('',(0.,-1.,0.));
#6755=DIRECTION('',(-1.,0.,-2.40370335797945E-16));
#6756=DIRECTION('center_axis',(0.866025403784439,0.,0.5));
#6757=DIRECTION('ref_axis',(-0.5,0.,0.866025403784439));
#6758=DIRECTION('',(0.5,0.,-0.866025403784439));
#6759=DIRECTION('',(-0.5,0.,0.866025403784439));
#6760=DIRECTION('center_axis',(0.,1.,0.));
#6761=DIRECTION('ref_axis',(1.,0.,0.));
#6762=DIRECTION('center_axis',(0.,-1.,0.));
#6763=DIRECTION('ref_axis',(0.,0.,-1.));
#6764=DIRECTION('axis',(0.,0.,1.));
#6765=DIRECTION('refdir',(1.,0.,0.));
#6766=DIRECTION('axis',(0.,0.,1.));
#6767=DIRECTION('refdir',(1.,0.,0.));
#6768=DIRECTION('center_axis',(0.,1.,0.));
#6769=DIRECTION('ref_axis',(1.,0.,0.));
#6770=DIRECTION('center_axis',(0.,1.,0.));
#6771=DIRECTION('ref_axis',(1.,0.,0.));
#6772=DIRECTION('',(0.,1.,0.));
#6773=DIRECTION('center_axis',(0.,-1.,0.));
#6774=DIRECTION('ref_axis',(1.,0.,0.));
#6775=DIRECTION('center_axis',(0.,1.,0.));
#6776=DIRECTION('ref_axis',(1.,0.,0.));
#6777=DIRECTION('center_axis',(0.,1.,0.));
#6778=DIRECTION('ref_axis',(1.,0.,0.));
#6779=DIRECTION('center_axis',(0.,1.,0.));
#6780=DIRECTION('ref_axis',(1.,0.,0.));
#6781=DIRECTION('',(0.5,0.,-0.866025403784439));
#6782=DIRECTION('',(-0.5,0.,-0.866025403784439));
#6783=DIRECTION('',(-1.,0.,-1.60246890531964E-16));
#6784=DIRECTION('',(-0.5,0.,0.866025403784439));
#6785=DIRECTION('',(0.5,0.,0.866025403784439));
#6786=DIRECTION('',(1.,0.,1.60246890531964E-16));
#6787=DIRECTION('center_axis',(0.,-1.,0.));
#6788=DIRECTION('ref_axis',(1.,0.,0.));
#6789=DIRECTION('center_axis',(0.,1.,0.));
#6790=DIRECTION('ref_axis',(1.,0.,0.));
#6791=DIRECTION('',(0.5,0.,-0.866025403784439));
#6792=DIRECTION('',(1.,0.,1.60246890531964E-16));
#6793=DIRECTION('',(0.5,0.,0.866025403784439));
#6794=DIRECTION('',(-0.5,0.,0.866025403784439));
#6795=DIRECTION('',(-1.,0.,-1.60246890531964E-16));
#6796=DIRECTION('',(-0.5,0.,-0.866025403784439));
#6797=DIRECTION('center_axis',(0.,-1.,0.));
#6798=DIRECTION('ref_axis',(1.,0.,0.));
#6799=DIRECTION('center_axis',(-1.60246890531964E-16,0.,1.));
#6800=DIRECTION('ref_axis',(1.,0.,1.60246890531964E-16));
#6801=DIRECTION('',(0.,1.,0.));
#6802=DIRECTION('',(0.,1.,0.));
#6803=DIRECTION('center_axis',(-0.866025403784439,0.,0.5));
#6804=DIRECTION('ref_axis',(0.5,0.,0.866025403784439));
#6805=DIRECTION('',(0.,1.,0.));
#6806=DIRECTION('center_axis',(-0.866025403784439,0.,-0.5));
#6807=DIRECTION('ref_axis',(-0.5,0.,0.866025403784439));
#6808=DIRECTION('',(0.,1.,0.));
#6809=DIRECTION('center_axis',(1.60246890531964E-16,0.,-1.));
#6810=DIRECTION('ref_axis',(-1.,0.,-1.60246890531964E-16));
#6811=DIRECTION('',(0.,1.,0.));
#6812=DIRECTION('center_axis',(0.866025403784439,0.,-0.5));
#6813=DIRECTION('ref_axis',(-0.5,0.,-0.866025403784439));
#6814=DIRECTION('',(0.,1.,0.));
#6815=DIRECTION('center_axis',(0.866025403784439,0.,0.5));
#6816=DIRECTION('ref_axis',(0.5,0.,-0.866025403784439));
#6817=DIRECTION('center_axis',(0.,1.,0.));
#6818=DIRECTION('ref_axis',(0.,0.,1.));
#6819=DIRECTION('center_axis',(0.,-1.,0.));
#6820=DIRECTION('ref_axis',(1.,0.,0.));
#6821=DIRECTION('center_axis',(0.,-1.,0.));
#6822=DIRECTION('ref_axis',(1.,0.,0.));
#6823=DIRECTION('',(0.,1.,0.));
#6824=DIRECTION('center_axis',(0.,-1.,0.));
#6825=DIRECTION('ref_axis',(1.,0.,0.));
#6826=DIRECTION('center_axis',(0.,1.,0.));
#6827=DIRECTION('ref_axis',(0.,0.,1.));
#6828=DIRECTION('center_axis',(0.,-1.,0.));
#6829=DIRECTION('ref_axis',(1.,0.,0.));
#6830=DIRECTION('center_axis',(0.,-1.,0.));
#6831=DIRECTION('ref_axis',(1.,0.,0.));
#6832=DIRECTION('',(0.,1.,0.));
#6833=DIRECTION('center_axis',(0.,-1.,0.));
#6834=DIRECTION('ref_axis',(1.,0.,0.));
#6835=DIRECTION('center_axis',(0.,-1.,0.));
#6836=DIRECTION('ref_axis',(1.,0.,0.));
#6837=DIRECTION('',(0.,1.,0.));
#6838=DIRECTION('center_axis',(0.,-1.,0.));
#6839=DIRECTION('ref_axis',(0.,0.,-1.));
#6840=DIRECTION('center_axis',(0.,-1.,0.));
#6841=DIRECTION('ref_axis',(1.,0.,0.));
#6842=DIRECTION('center_axis',(0.,-1.,0.));
#6843=DIRECTION('ref_axis',(1.,0.,0.));
#6844=DIRECTION('',(0.,1.,0.));
#6845=DIRECTION('axis',(0.,0.,1.));
#6846=DIRECTION('refdir',(1.,0.,0.));
#6847=DIRECTION('center_axis',(0.,1.,0.));
#6848=DIRECTION('ref_axis',(0.,0.,1.));
#6849=DIRECTION('center_axis',(0.,-1.,0.));
#6850=DIRECTION('ref_axis',(1.,0.,0.));
#6851=DIRECTION('center_axis',(0.,-1.,0.));
#6852=DIRECTION('ref_axis',(1.,0.,0.));
#6853=DIRECTION('center_axis',(0.,-1.,0.));
#6854=DIRECTION('ref_axis',(1.,0.,0.));
#6855=DIRECTION('center_axis',(0.,-1.,0.));
#6856=DIRECTION('ref_axis',(1.,0.,0.));
#6857=DIRECTION('',(0.,1.,0.));
#6858=DIRECTION('center_axis',(0.,-1.,0.));
#6859=DIRECTION('ref_axis',(0.,0.,-1.));
#6860=DIRECTION('center_axis',(0.,-1.,0.));
#6861=DIRECTION('ref_axis',(1.,0.,0.));
#6862=DIRECTION('center_axis',(0.,-1.,0.));
#6863=DIRECTION('ref_axis',(1.,0.,0.));
#6864=DIRECTION('center_axis',(0.,-1.,0.));
#6865=DIRECTION('ref_axis',(1.,0.,0.));
#6866=DIRECTION('',(0.,1.,0.));
#6867=DIRECTION('center_axis',(0.,-1.,0.));
#6868=DIRECTION('ref_axis',(0.,0.,-1.));
#6869=DIRECTION('center_axis',(0.,-1.,0.));
#6870=DIRECTION('ref_axis',(1.,0.,0.));
#6871=DIRECTION('center_axis',(0.,-1.,0.));
#6872=DIRECTION('ref_axis',(1.,0.,0.));
#6873=DIRECTION('',(0.,1.,0.));
#6874=DIRECTION('',(0.,0.,1.));
#6875=DIRECTION('',(1.,0.,0.));
#6876=DIRECTION('',(0.,0.,1.));
#6877=DIRECTION('',(1.,0.,0.));
#6878=DIRECTION('axis',(0.,0.,1.));
#6879=DIRECTION('refdir',(1.,0.,0.));
#6880=DIRECTION('center_axis',(0.,-1.,0.));
#6881=DIRECTION('ref_axis',(0.,0.,-1.));
#6882=DIRECTION('center_axis',(-1.,0.,-1.22464679914735E-16));
#6883=DIRECTION('ref_axis',(-1.22464679914735E-16,0.,1.));
#6884=DIRECTION('center_axis',(0.,1.,0.));
#6885=DIRECTION('ref_axis',(0.,0.,-1.));
#6886=DIRECTION('axis',(0.,0.,1.));
#6887=DIRECTION('refdir',(1.,0.,0.));
#6888=DIRECTION('center_axis',(0.,1.,0.));
#6889=DIRECTION('ref_axis',(1.,0.,0.));
#6890=DIRECTION('center_axis',(0.,1.,0.));
#6891=DIRECTION('ref_axis',(1.,0.,0.));
#6892=DIRECTION('',(0.,1.,0.));
#6893=DIRECTION('center_axis',(0.,1.,0.));
#6894=DIRECTION('ref_axis',(1.,0.,0.));
#6895=DIRECTION('center_axis',(0.,1.,0.));
#6896=DIRECTION('ref_axis',(1.,0.,0.));
#6897=DIRECTION('center_axis',(0.,-1.,0.));
#6898=DIRECTION('ref_axis',(1.,0.,0.));
#6899=DIRECTION('center_axis',(0.,1.,0.));
#6900=DIRECTION('ref_axis',(1.,0.,0.));
#6901=DIRECTION('center_axis',(0.,1.,0.));
#6902=DIRECTION('ref_axis',(1.,0.,0.));
#6903=DIRECTION('center_axis',(0.,1.,0.));
#6904=DIRECTION('ref_axis',(1.,0.,0.));
#6905=DIRECTION('',(0.,-1.,0.));
#6906=DIRECTION('center_axis',(0.,-1.,0.));
#6907=DIRECTION('ref_axis',(1.,0.,0.));
#6908=DIRECTION('center_axis',(0.,1.,0.));
#6909=DIRECTION('ref_axis',(1.,0.,0.));
#6910=DIRECTION('center_axis',(0.,-1.,0.));
#6911=DIRECTION('ref_axis',(1.,0.,0.));
#6912=DIRECTION('',(0.,-1.,0.));
#6913=DIRECTION('center_axis',(0.,1.,0.));
#6914=DIRECTION('ref_axis',(1.,0.,0.));
#6915=DIRECTION('center_axis',(0.,1.,0.));
#6916=DIRECTION('ref_axis',(1.,0.,0.));
#6917=DIRECTION('',(0.,-1.,0.));
#6918=DIRECTION('center_axis',(0.,1.,0.));
#6919=DIRECTION('ref_axis',(1.,0.,0.));
#6920=DIRECTION('center_axis',(0.,1.,0.));
#6921=DIRECTION('ref_axis',(1.,0.,0.));
#6922=DIRECTION('center_axis',(0.,1.,0.));
#6923=DIRECTION('ref_axis',(1.,0.,0.));
#6924=DIRECTION('axis',(0.,0.,1.));
#6925=DIRECTION('refdir',(1.,0.,0.));
#6926=DIRECTION('center_axis',(0.,-1.,0.));
#6927=DIRECTION('ref_axis',(0.,0.,-1.));
#6928=DIRECTION('center_axis',(-1.,0.,-1.22464679914735E-16));
#6929=DIRECTION('ref_axis',(-1.22464679914735E-16,0.,1.));
#6930=DIRECTION('center_axis',(0.,1.,0.));
#6931=DIRECTION('ref_axis',(0.,0.,-1.));
#6932=DIRECTION('axis',(0.,0.,1.));
#6933=DIRECTION('refdir',(1.,0.,0.));
#6934=DIRECTION('center_axis',(0.,1.,0.));
#6935=DIRECTION('ref_axis',(1.,0.,0.));
#6936=DIRECTION('center_axis',(0.,1.,0.));
#6937=DIRECTION('ref_axis',(1.,0.,0.));
#6938=DIRECTION('',(0.,-1.,0.));
#6939=DIRECTION('center_axis',(0.,1.,0.));
#6940=DIRECTION('ref_axis',(1.,0.,0.));
#6941=DIRECTION('center_axis',(0.,1.,0.));
#6942=DIRECTION('ref_axis',(1.,0.,0.));
#6943=DIRECTION('center_axis',(0.,1.,0.));
#6944=DIRECTION('ref_axis',(1.,0.,0.));
#6945=DIRECTION('axis',(0.,0.,1.));
#6946=DIRECTION('refdir',(1.,0.,0.));
#6947=DIRECTION('center_axis',(0.,1.,0.));
#6948=DIRECTION('ref_axis',(1.,0.,0.));
#6949=DIRECTION('center_axis',(0.,1.,0.));
#6950=DIRECTION('ref_axis',(1.,0.,0.));
#6951=DIRECTION('',(0.707106781186548,-0.707106781186547,-8.65956056235494E-17));
#6952=DIRECTION('center_axis',(0.,-1.,0.));
#6953=DIRECTION('ref_axis',(1.,0.,0.));
#6954=DIRECTION('center_axis',(0.,1.,0.));
#6955=DIRECTION('ref_axis',(1.,0.,0.));
#6956=DIRECTION('',(0.,-1.,0.));
#6957=DIRECTION('center_axis',(0.,-1.,0.));
#6958=DIRECTION('ref_axis',(1.,0.,0.));
#6959=DIRECTION('center_axis',(0.,1.,0.));
#6960=DIRECTION('ref_axis',(1.,0.,0.));
#6961=DIRECTION('center_axis',(0.,1.,0.));
#6962=DIRECTION('ref_axis',(1.,0.,0.));
#6963=DIRECTION('center_axis',(0.,1.,0.));
#6964=DIRECTION('ref_axis',(1.,0.,0.));
#6965=DIRECTION('',(0.,-1.,0.));
#6966=DIRECTION('center_axis',(0.,1.,0.));
#6967=DIRECTION('ref_axis',(1.,0.,0.));
#6968=DIRECTION('center_axis',(0.,1.,0.));
#6969=DIRECTION('ref_axis',(1.,0.,0.));
#6970=DIRECTION('axis',(0.,0.,1.));
#6971=DIRECTION('refdir',(1.,0.,0.));
#6972=DIRECTION('center_axis',(0.,1.,0.));
#6973=DIRECTION('ref_axis',(1.,0.,0.));
#6974=DIRECTION('',(0.866025403784439,-0.5,1.06057523872491E-16));
#6975=DIRECTION('center_axis',(0.,-1.,0.));
#6976=DIRECTION('ref_axis',(1.,0.,0.));
#6977=DIRECTION('center_axis',(0.,-1.,0.));
#6978=DIRECTION('ref_axis',(1.,0.,0.));
#6979=DIRECTION('center_axis',(0.,1.,0.));
#6980=DIRECTION('ref_axis',(1.,0.,0.));
#6981=DIRECTION('',(-0.866025403784439,-0.5,-1.06057523872491E-16));
#6982=DIRECTION('center_axis',(1.20185167898973E-16,0.,-1.));
#6983=DIRECTION('ref_axis',(-1.,0.,-1.20185167898973E-16));
#6984=DIRECTION('',(0.,1.,0.));
#6985=DIRECTION('',(0.,1.,0.));
#6986=DIRECTION('center_axis',(-0.866025403784439,0.,-0.5));
#6987=DIRECTION('ref_axis',(-0.5,0.,0.866025403784439));
#6988=DIRECTION('',(0.,1.,0.));
#6989=DIRECTION('center_axis',(-0.866025403784439,0.,0.5));
#6990=DIRECTION('ref_axis',(0.5,0.,0.866025403784439));
#6991=DIRECTION('',(0.,1.,0.));
#6992=DIRECTION('center_axis',(0.,1.,0.));
#6993=DIRECTION('ref_axis',(1.,0.,0.));
#6994=DIRECTION('center_axis',(0.,1.,0.));
#6995=DIRECTION('ref_axis',(1.,0.,0.));
#6996=DIRECTION('',(0.,-1.,0.));
#6997=DIRECTION('center_axis',(0.,1.,0.));
#6998=DIRECTION('ref_axis',(1.,0.,0.));
#6999=DIRECTION('center_axis',(-2.40370335797945E-16,0.,1.));
#7000=DIRECTION('ref_axis',(1.,0.,2.40370335797945E-16));
#7001=DIRECTION('',(0.,1.,0.));
#7002=DIRECTION('center_axis',(0.866025403784439,0.,-0.5));
#7003=DIRECTION('ref_axis',(-0.5,0.,-0.866025403784439));
#7004=DIRECTION('',(0.,1.,0.));
#7005=DIRECTION('center_axis',(0.866025403784439,0.,0.5));
#7006=DIRECTION('ref_axis',(0.5,0.,-0.866025403784439));
#7007=DIRECTION('center_axis',(0.,1.,0.));
#7008=DIRECTION('ref_axis',(1.,0.,0.));
#7009=DIRECTION('center_axis',(0.,1.,0.));
#7010=DIRECTION('ref_axis',(1.,0.,0.));
#7011=DIRECTION('',(0.,0.,1.));
#7012=DIRECTION('',(1.,0.,0.));
#7013=DIRECTION('',(0.,0.,1.));
#7014=DIRECTION('',(1.,0.,0.));
#7015=DIRECTION('',(0.,0.,1.));
#7016=DIRECTION('',(1.,0.,0.));
#7017=DIRECTION('',(0.,0.,1.));
#7018=DIRECTION('',(1.,0.,0.));
#7019=DIRECTION('',(0.,0.,1.));
#7020=DIRECTION('',(1.,0.,0.));
#7021=DIRECTION('',(0.,0.,1.));
#7022=DIRECTION('',(1.,0.,0.));
#7023=DIRECTION('',(0.,0.,1.));
#7024=DIRECTION('',(1.,0.,0.));
#7025=DIRECTION('',(0.,0.,1.));
#7026=DIRECTION('',(1.,0.,0.));
#7027=DIRECTION('',(0.,0.,1.));
#7028=DIRECTION('',(1.,0.,0.));
#7029=DIRECTION('',(0.,0.,1.));
#7030=DIRECTION('',(1.,0.,0.));
#7031=DIRECTION('',(0.,1.,2.22044604925031E-16));
#7032=DIRECTION('',(1.,0.,0.));
#7033=DIRECTION('',(0.,1.,2.22044604925031E-16));
#7034=DIRECTION('',(1.,0.,0.));
#7035=DIRECTION('',(0.,0.,1.));
#7036=DIRECTION('',(2.22044604925031E-16,-1.,0.));
#7037=DIRECTION('',(0.,-1.,2.22044604925031E-16));
#7038=DIRECTION('',(1.,0.,0.));
#7039=DIRECTION('',(0.,0.,1.));
#7040=DIRECTION('',(-1.,1.22464679914735E-16,0.));
#7041=DIRECTION('',(0.,1.,2.22044604925031E-16));
#7042=DIRECTION('',(1.,0.,0.));
#7043=DIRECTION('',(0.,1.,2.22044604925031E-16));
#7044=DIRECTION('',(1.,0.,0.));
#7045=DIRECTION('',(0.,0.,1.));
#7046=DIRECTION('',(2.22044604925031E-16,-1.,0.));
#7047=DIRECTION('',(0.,-1.,2.22044604925031E-16));
#7048=DIRECTION('',(1.,0.,0.));
#7049=DIRECTION('',(0.,0.,1.));
#7050=DIRECTION('',(1.,0.,0.));
#7051=DIRECTION('',(0.,0.,1.));
#7052=DIRECTION('',(1.,0.,0.));
#7053=DIRECTION('',(0.,0.,1.));
#7054=DIRECTION('',(1.,0.,0.));
#7055=DIRECTION('',(0.,0.,1.));
#7056=DIRECTION('',(-1.,1.22464679914735E-16,0.));
#7057=DIRECTION('',(0.,0.,1.));
#7058=DIRECTION('',(1.,0.,0.));
#7059=DIRECTION('',(0.,0.,1.));
#7060=DIRECTION('',(1.,0.,0.));
#7061=DIRECTION('',(0.,0.,1.));
#7062=DIRECTION('',(1.,0.,0.));
#7063=DIRECTION('',(0.,0.,1.));
#7064=DIRECTION('',(1.,0.,0.));
#7065=DIRECTION('',(0.,0.,1.));
#7066=DIRECTION('',(-1.,1.22464679914735E-16,0.));
#7067=DIRECTION('',(0.,0.,1.));
#7068=DIRECTION('',(1.,0.,0.));
#7069=DIRECTION('',(0.,0.,1.));
#7070=DIRECTION('',(1.,0.,0.));
#7071=DIRECTION('',(0.,0.,1.));
#7072=DIRECTION('',(1.,0.,0.));
#7073=DIRECTION('',(0.,0.,1.));
#7074=DIRECTION('',(1.,0.,0.));
#7075=DIRECTION('',(0.,0.,1.));
#7076=DIRECTION('',(-1.,1.22464679914735E-16,0.));
#7077=DIRECTION('',(0.,0.,1.));
#7078=DIRECTION('',(1.,0.,0.));
#7079=DIRECTION('',(0.,0.,1.));
#7080=DIRECTION('',(1.,0.,0.));
#7081=DIRECTION('',(0.,0.,1.));
#7082=DIRECTION('',(1.,0.,0.));
#7083=DIRECTION('',(0.,0.,1.));
#7084=DIRECTION('',(1.,0.,0.));
#7085=DIRECTION('',(0.,0.,1.));
#7086=DIRECTION('',(-1.,1.22464679914735E-16,0.));
#7087=DIRECTION('',(0.,0.,1.));
#7088=DIRECTION('',(1.,0.,0.));
#7089=DIRECTION('',(0.,0.,1.));
#7090=DIRECTION('',(1.,0.,0.));
#7091=DIRECTION('',(0.,0.,1.));
#7092=DIRECTION('',(1.,0.,0.));
#7093=DIRECTION('axis',(0.,0.,1.));
#7094=DIRECTION('refdir',(1.,0.,0.));
#7095=DIRECTION('axis',(0.,0.,1.));
#7096=DIRECTION('refdir',(1.,0.,0.));
#7097=DIRECTION('center_axis',(0.,1.,0.));
#7098=DIRECTION('ref_axis',(1.,0.,0.));
#7099=DIRECTION('center_axis',(0.,1.,0.));
#7100=DIRECTION('ref_axis',(1.,0.,0.));
#7101=DIRECTION('',(0.,1.,0.));
#7102=DIRECTION('center_axis',(0.,-1.,0.));
#7103=DIRECTION('ref_axis',(1.,0.,0.));
#7104=DIRECTION('center_axis',(0.,1.,0.));
#7105=DIRECTION('ref_axis',(1.,0.,0.));
#7106=DIRECTION('center_axis',(0.,1.,0.));
#7107=DIRECTION('ref_axis',(1.,0.,0.));
#7108=DIRECTION('center_axis',(0.,1.,0.));
#7109=DIRECTION('ref_axis',(1.,0.,0.));
#7110=DIRECTION('center_axis',(0.,-1.,0.));
#7111=DIRECTION('ref_axis',(1.,0.,0.));
#7112=DIRECTION('',(0.,1.,0.));
#7113=DIRECTION('center_axis',(0.,-1.,0.));
#7114=DIRECTION('ref_axis',(1.,0.,0.));
#7115=DIRECTION('center_axis',(0.,1.,0.));
#7116=DIRECTION('ref_axis',(1.,0.,0.));
#7117=DIRECTION('center_axis',(0.,1.,0.));
#7118=DIRECTION('ref_axis',(1.,0.,0.));
#7119=DIRECTION('center_axis',(0.,1.,0.));
#7120=DIRECTION('ref_axis',(1.,0.,0.));
#7121=DIRECTION('center_axis',(0.,-1.,0.));
#7122=DIRECTION('ref_axis',(1.,0.,0.));
#7123=DIRECTION('center_axis',(0.,1.,0.));
#7124=DIRECTION('ref_axis',(1.,0.,0.));
#7125=DIRECTION('',(0.,-1.,0.));
#7126=DIRECTION('center_axis',(0.,1.,0.));
#7127=DIRECTION('ref_axis',(1.,0.,0.));
#7128=DIRECTION('center_axis',(0.,1.,0.));
#7129=DIRECTION('ref_axis',(1.,0.,0.));
#7130=DIRECTION('',(0.,-1.,0.));
#7131=DIRECTION('center_axis',(0.,-1.,0.));
#7132=DIRECTION('ref_axis',(1.,0.,0.));
#7133=DIRECTION('center_axis',(0.,1.,0.));
#7134=DIRECTION('ref_axis',(1.,0.,0.));
#7135=DIRECTION('center_axis',(0.,1.,0.));
#7136=DIRECTION('ref_axis',(1.,0.,0.));
#7137=DIRECTION('',(0.,-1.,0.));
#7138=DIRECTION('center_axis',(0.,1.,0.));
#7139=DIRECTION('ref_axis',(1.,0.,0.));
#7140=DIRECTION('center_axis',(0.,1.,0.));
#7141=DIRECTION('ref_axis',(1.,0.,0.));
#7142=DIRECTION('axis',(0.,0.,1.));
#7143=DIRECTION('refdir',(1.,0.,0.));
#7144=DIRECTION('center_axis',(0.,-1.,0.));
#7145=DIRECTION('ref_axis',(0.,0.,-1.));
#7146=DIRECTION('center_axis',(-1.,0.,-1.22464679914735E-16));
#7147=DIRECTION('ref_axis',(-1.22464679914735E-16,0.,1.));
#7148=DIRECTION('center_axis',(0.,1.,0.));
#7149=DIRECTION('ref_axis',(0.,0.,-1.));
#7150=DIRECTION('axis',(0.,0.,1.));
#7151=DIRECTION('refdir',(1.,0.,0.));
#7152=DIRECTION('center_axis',(0.,1.,0.));
#7153=DIRECTION('ref_axis',(1.,0.,0.));
#7154=DIRECTION('center_axis',(0.,1.,0.));
#7155=DIRECTION('ref_axis',(1.,0.,0.));
#7156=DIRECTION('',(0.,1.,0.));
#7157=DIRECTION('center_axis',(0.,-1.,0.));
#7158=DIRECTION('ref_axis',(1.,0.,0.));
#7159=DIRECTION('center_axis',(0.,1.,0.));
#7160=DIRECTION('ref_axis',(1.,0.,0.));
#7161=DIRECTION('center_axis',(0.,1.,0.));
#7162=DIRECTION('ref_axis',(1.,0.,0.));
#7163=DIRECTION('center_axis',(0.,1.,0.));
#7164=DIRECTION('ref_axis',(1.,0.,0.));
#7165=DIRECTION('',(0.,-1.,0.));
#7166=DIRECTION('center_axis',(0.,1.,0.));
#7167=DIRECTION('ref_axis',(1.,0.,0.));
#7168=DIRECTION('center_axis',(0.,1.,0.));
#7169=DIRECTION('ref_axis',(1.,0.,0.));
#7170=DIRECTION('center_axis',(0.,1.,0.));
#7171=DIRECTION('ref_axis',(1.,0.,0.));
#7172=DIRECTION('axis',(0.,0.,1.));
#7173=DIRECTION('refdir',(1.,0.,0.));
#7174=DIRECTION('center_axis',(0.,1.,0.));
#7175=DIRECTION('ref_axis',(0.,0.,1.));
#7176=DIRECTION('center_axis',(0.,-1.,0.));
#7177=DIRECTION('ref_axis',(1.,0.,0.));
#7178=DIRECTION('center_axis',(0.,-1.,0.));
#7179=DIRECTION('ref_axis',(1.,0.,0.));
#7180=DIRECTION('center_axis',(0.,-1.,0.));
#7181=DIRECTION('ref_axis',(1.,0.,0.));
#7182=DIRECTION('',(0.707106781186547,0.707106781186548,8.65956056235493E-17));
#7183=DIRECTION('center_axis',(0.,-1.,0.));
#7184=DIRECTION('ref_axis',(1.,0.,0.));
#7185=DIRECTION('center_axis',(0.,-1.,0.));
#7186=DIRECTION('ref_axis',(1.,0.,0.));
#7187=DIRECTION('',(0.,1.,0.));
#7188=DIRECTION('center_axis',(0.,1.,0.));
#7189=DIRECTION('ref_axis',(1.,0.,0.));
#7190=DIRECTION('center_axis',(0.,-1.,0.));
#7191=DIRECTION('ref_axis',(1.,0.,0.));
#7192=DIRECTION('',(-0.707106781186547,0.707106781186548,-8.65956056235493E-17));
#7193=DIRECTION('center_axis',(0.,-1.,0.));
#7194=DIRECTION('ref_axis',(0.,0.,-1.));
#7195=DIRECTION('center_axis',(0.,-1.,0.));
#7196=DIRECTION('ref_axis',(1.,0.,0.));
#7197=DIRECTION('center_axis',(0.,1.,0.));
#7198=DIRECTION('ref_axis',(1.,0.,0.));
#7199=DIRECTION('center_axis',(0.,1.,0.));
#7200=DIRECTION('ref_axis',(1.,0.,0.));
#7201=DIRECTION('',(-0.447213595499958,0.894427190999916,-5.47678698264203E-17));
#7202=DIRECTION('center_axis',(0.,-1.,0.));
#7203=DIRECTION('ref_axis',(1.,0.,0.));
#7204=DIRECTION('center_axis',(0.,1.,0.));
#7205=DIRECTION('ref_axis',(1.,0.,0.));
#7206=DIRECTION('',(0.,1.,0.));
#7207=DIRECTION('center_axis',(0.,1.,0.));
#7208=DIRECTION('ref_axis',(1.,0.,0.));
#7209=DIRECTION('center_axis',(0.,-1.,0.));
#7210=DIRECTION('ref_axis',(1.,0.,0.));
#7211=DIRECTION('',(-0.707106781186547,0.707106781186548,-8.65956056235493E-17));
#7212=DIRECTION('center_axis',(0.,-1.,0.));
#7213=DIRECTION('ref_axis',(0.,0.,-1.));
#7214=DIRECTION('center_axis',(0.866025403784439,0.,-0.5));
#7215=DIRECTION('ref_axis',(0.5,0.,0.866025403784439));
#7216=DIRECTION('',(-0.5,0.,-0.866025403784439));
#7217=DIRECTION('',(0.,-1.,0.));
#7218=DIRECTION('',(0.5,0.,0.866025403784439));
#7219=DIRECTION('',(0.,-1.,0.));
#7220=DIRECTION('center_axis',(1.60246890531964E-16,0.,-1.));
#7221=DIRECTION('ref_axis',(1.,0.,1.60246890531964E-16));
#7222=DIRECTION('',(-1.,0.,-1.60246890531964E-16));
#7223=DIRECTION('',(0.,-1.,0.));
#7224=DIRECTION('',(1.,0.,1.60246890531964E-16));
#7225=DIRECTION('center_axis',(-0.866025403784439,0.,-0.5));
#7226=DIRECTION('ref_axis',(0.5,0.,-0.866025403784439));
#7227=DIRECTION('',(-0.5,0.,0.866025403784439));
#7228=DIRECTION('',(0.,-1.,0.));
#7229=DIRECTION('',(0.5,0.,-0.866025403784439));
#7230=DIRECTION('center_axis',(-0.866025403784439,0.,0.5));
#7231=DIRECTION('ref_axis',(-0.5,0.,-0.866025403784439));
#7232=DIRECTION('',(0.5,0.,0.866025403784439));
#7233=DIRECTION('',(0.,-1.,0.));
#7234=DIRECTION('',(-0.5,0.,-0.866025403784439));
#7235=DIRECTION('center_axis',(-1.60246890531964E-16,0.,1.));
#7236=DIRECTION('ref_axis',(-1.,0.,-1.60246890531964E-16));
#7237=DIRECTION('',(1.,0.,1.60246890531964E-16));
#7238=DIRECTION('',(0.,-1.,0.));
#7239=DIRECTION('',(-1.,0.,-1.60246890531964E-16));
#7240=DIRECTION('center_axis',(0.866025403784439,0.,0.5));
#7241=DIRECTION('ref_axis',(-0.5,0.,0.866025403784439));
#7242=DIRECTION('',(0.5,0.,-0.866025403784439));
#7243=DIRECTION('',(-0.5,0.,0.866025403784439));
#7244=DIRECTION('center_axis',(0.,1.,0.));
#7245=DIRECTION('ref_axis',(1.,0.,0.));
#7246=DIRECTION('center_axis',(0.,-1.,0.));
#7247=DIRECTION('ref_axis',(0.,0.,-1.));
#7248=DIRECTION('axis',(0.,0.,1.));
#7249=DIRECTION('refdir',(1.,0.,0.));
#7250=DIRECTION('center_axis',(1.,0.,0.));
#7251=DIRECTION('ref_axis',(0.,0.,-1.));
#7252=DIRECTION('center_axis',(1.,0.,0.));
#7253=DIRECTION('ref_axis',(0.,0.,-1.));
#7254=DIRECTION('',(1.,0.,0.));
#7255=DIRECTION('center_axis',(-1.,0.,0.));
#7256=DIRECTION('ref_axis',(0.,0.,-1.));
#7257=DIRECTION('center_axis',(1.,0.,0.));
#7258=DIRECTION('ref_axis',(0.,0.,-1.));
#7259=DIRECTION('center_axis',(1.,0.,0.));
#7260=DIRECTION('ref_axis',(0.,0.,-1.));
#7261=DIRECTION('',(1.,0.,0.));
#7262=DIRECTION('center_axis',(-1.,0.,0.));
#7263=DIRECTION('ref_axis',(0.,0.,-1.));
#7264=DIRECTION('center_axis',(0.,0.,1.));
#7265=DIRECTION('ref_axis',(1.,0.,0.));
#7266=DIRECTION('',(0.,1.,0.));
#7267=DIRECTION('center_axis',(0.,0.,1.));
#7268=DIRECTION('ref_axis',(1.,0.,0.));
#7269=DIRECTION('center_axis',(0.,0.,1.));
#7270=DIRECTION('ref_axis',(1.,0.,0.));
#7271=DIRECTION('center_axis',(0.,0.,1.));
#7272=DIRECTION('ref_axis',(1.,0.,0.));
#7273=DIRECTION('',(0.,0.,1.));
#7274=DIRECTION('center_axis',(0.,0.,-1.));
#7275=DIRECTION('ref_axis',(1.,0.,0.));
#7276=DIRECTION('center_axis',(0.,0.,1.));
#7277=DIRECTION('ref_axis',(1.,0.,0.));
#7278=DIRECTION('center_axis',(0.,0.,1.));
#7279=DIRECTION('ref_axis',(1.,0.,0.));
#7280=DIRECTION('',(0.,-1.,0.));
#7281=DIRECTION('center_axis',(0.,1.,0.));
#7282=DIRECTION('ref_axis',(1.,0.,0.));
#7283=DIRECTION('center_axis',(0.,1.,0.));
#7284=DIRECTION('ref_axis',(1.,0.,0.));
#7285=DIRECTION('',(0.,1.,0.));
#7286=DIRECTION('center_axis',(0.,-1.,0.));
#7287=DIRECTION('ref_axis',(1.,0.,0.));
#7288=DIRECTION('center_axis',(1.,0.,0.));
#7289=DIRECTION('ref_axis',(0.,1.,0.));
#7290=DIRECTION('',(0.,-1.,0.));
#7291=DIRECTION('',(0.,0.,1.));
#7292=DIRECTION('',(0.,1.,0.));
#7293=DIRECTION('',(0.,0.,-1.));
#7294=DIRECTION('center_axis',(0.,1.,0.));
#7295=DIRECTION('ref_axis',(-1.,0.,0.));
#7296=DIRECTION('',(1.,0.,0.));
#7297=DIRECTION('',(0.,0.,1.));
#7298=DIRECTION('',(-1.,0.,0.));
#7299=DIRECTION('center_axis',(-1.,0.,0.));
#7300=DIRECTION('ref_axis',(0.,-1.,0.));
#7301=DIRECTION('',(0.,1.,0.));
#7302=DIRECTION('',(0.,0.,1.));
#7303=DIRECTION('',(0.,-1.,0.));
#7304=DIRECTION('center_axis',(0.,0.,1.));
#7305=DIRECTION('ref_axis',(1.,0.,0.));
#7306=DIRECTION('',(1.,0.,0.));
#7307=DIRECTION('',(0.,-1.,0.));
#7308=DIRECTION('',(-1.,0.,0.));
#7309=DIRECTION('',(0.,1.,0.));
#7310=DIRECTION('',(1.,0.,0.));
#7311=DIRECTION('center_axis',(0.,-1.,0.));
#7312=DIRECTION('ref_axis',(1.,0.,0.));
#7313=DIRECTION('',(1.,0.,0.));
#7314=DIRECTION('',(0.,0.,1.));
#7315=DIRECTION('center_axis',(0.,-1.,0.));
#7316=DIRECTION('ref_axis',(1.,0.,0.));
#7317=DIRECTION('',(0.,0.,1.));
#7318=DIRECTION('',(1.,0.,0.));
#7319=DIRECTION('center_axis',(0.,1.,0.));
#7320=DIRECTION('ref_axis',(-1.,0.,0.));
#7321=DIRECTION('',(0.,0.,1.));
#7322=DIRECTION('',(-1.,0.,0.));
#7323=DIRECTION('',(0.,0.,1.));
#7324=DIRECTION('center_axis',(1.,0.,0.));
#7325=DIRECTION('ref_axis',(0.,1.,0.));
#7326=DIRECTION('',(0.,1.,0.));
#7327=DIRECTION('center_axis',(-1.,0.,0.));
#7328=DIRECTION('ref_axis',(0.,-1.,0.));
#7329=DIRECTION('',(0.,-1.,0.));
#7330=DIRECTION('center_axis',(0.,0.,1.));
#7331=DIRECTION('ref_axis',(1.,0.,0.));
#7332=DIRECTION('axis',(0.,0.,1.));
#7333=DIRECTION('refdir',(1.,0.,0.));
#7334=DIRECTION('center_axis',(0.866025403784439,0.,-0.5));
#7335=DIRECTION('ref_axis',(0.5,0.,0.866025403784439));
#7336=DIRECTION('',(0.5,0.,0.866025403784439));
#7337=DIRECTION('',(0.,-1.,0.));
#7338=DIRECTION('',(0.5,0.,0.866025403784439));
#7339=DIRECTION('',(0.,-1.,0.));
#7340=DIRECTION('center_axis',(1.20185167898973E-16,0.,-1.));
#7341=DIRECTION('ref_axis',(1.,0.,1.20185167898973E-16));
#7342=DIRECTION('',(1.,0.,1.20185167898973E-16));
#7343=DIRECTION('',(0.,-1.,0.));
#7344=DIRECTION('',(1.,0.,1.20185167898973E-16));
#7345=DIRECTION('center_axis',(-0.866025403784439,0.,-0.5));
#7346=DIRECTION('ref_axis',(0.5,0.,-0.866025403784439));
#7347=DIRECTION('',(0.5,0.,-0.866025403784439));
#7348=DIRECTION('',(0.,-1.,0.));
#7349=DIRECTION('',(0.5,0.,-0.866025403784439));
#7350=DIRECTION('center_axis',(-0.866025403784439,0.,0.5));
#7351=DIRECTION('ref_axis',(-0.5,0.,-0.866025403784439));
#7352=DIRECTION('',(-0.5,0.,-0.866025403784439));
#7353=DIRECTION('',(0.,-1.,0.));
#7354=DIRECTION('',(-0.5,0.,-0.866025403784439));
#7355=DIRECTION('center_axis',(-2.40370335797945E-16,0.,1.));
#7356=DIRECTION('ref_axis',(-1.,0.,-2.40370335797945E-16));
#7357=DIRECTION('',(-1.,0.,-2.40370335797945E-16));
#7358=DIRECTION('',(0.,-1.,0.));
#7359=DIRECTION('',(-1.,0.,-2.40370335797945E-16));
#7360=DIRECTION('center_axis',(0.866025403784439,0.,0.5));
#7361=DIRECTION('ref_axis',(-0.5,0.,0.866025403784439));
#7362=DIRECTION('',(-0.5,0.,0.866025403784439));
#7363=DIRECTION('',(-0.5,0.,0.866025403784439));
#7364=DIRECTION('center_axis',(0.,-1.,0.));
#7365=DIRECTION('ref_axis',(0.,0.,-1.));
#7366=DIRECTION('center_axis',(0.,1.,0.));
#7367=DIRECTION('ref_axis',(0.,0.,1.));
#7368=DIRECTION('center_axis',(0.,-1.,0.));
#7369=DIRECTION('ref_axis',(1.,0.,0.));
#7370=DIRECTION('center_axis',(0.,-1.,0.));
#7371=DIRECTION('ref_axis',(1.,0.,0.));
#7372=DIRECTION('center_axis',(0.,-1.,0.));
#7373=DIRECTION('ref_axis',(1.,0.,0.));
#7374=DIRECTION('',(0.707106781186548,0.707106781186547,8.65956056235494E-17));
#7375=DIRECTION('center_axis',(0.,-1.,0.));
#7376=DIRECTION('ref_axis',(1.,0.,0.));
#7377=DIRECTION('center_axis',(0.,1.,0.));
#7378=DIRECTION('ref_axis',(1.,0.,0.));
#7379=DIRECTION('',(0.,1.,0.));
#7380=DIRECTION('center_axis',(0.,1.,0.));
#7381=DIRECTION('ref_axis',(1.,0.,0.));
#7382=DIRECTION('center_axis',(0.,-1.,0.));
#7383=DIRECTION('ref_axis',(1.,0.,0.));
#7384=DIRECTION('',(-0.707106781186548,0.707106781186547,-8.65956056235494E-17));
#7385=DIRECTION('center_axis',(0.,-1.,0.));
#7386=DIRECTION('ref_axis',(0.,0.,-1.));
#7387=DIRECTION('axis',(0.,0.,1.));
#7388=DIRECTION('refdir',(1.,0.,0.));
#7389=DIRECTION('center_axis',(1.,0.,0.));
#7390=DIRECTION('ref_axis',(0.,0.,-1.));
#7391=DIRECTION('',(1.,0.,0.));
#7392=DIRECTION('center_axis',(0.,1.,0.));
#7393=DIRECTION('ref_axis',(0.,0.,1.));
#7394=DIRECTION('center_axis',(0.,-1.,0.));
#7395=DIRECTION('ref_axis',(1.,0.,0.));
#7396=DIRECTION('center_axis',(0.,-1.,0.));
#7397=DIRECTION('ref_axis',(1.,0.,0.));
#7398=DIRECTION('center_axis',(0.,-1.,0.));
#7399=DIRECTION('ref_axis',(1.,0.,0.));
#7400=DIRECTION('',(0.707106781186547,0.707106781186548,8.65956056235493E-17));
#7401=DIRECTION('center_axis',(0.,-1.,0.));
#7402=DIRECTION('ref_axis',(1.,0.,0.));
#7403=DIRECTION('center_axis',(0.,-1.,0.));
#7404=DIRECTION('ref_axis',(1.,0.,0.));
#7405=DIRECTION('',(0.,1.,0.));
#7406=DIRECTION('center_axis',(0.,-1.,0.));
#7407=DIRECTION('ref_axis',(0.,0.,-1.));
#7408=DIRECTION('center_axis',(0.,-1.,0.));
#7409=DIRECTION('ref_axis',(1.,0.,0.));
#7410=DIRECTION('center_axis',(0.,-1.,0.));
#7411=DIRECTION('ref_axis',(1.,0.,0.));
#7412=DIRECTION('center_axis',(0.,-1.,0.));
#7413=DIRECTION('ref_axis',(1.,0.,0.));
#7414=DIRECTION('',(0.,1.,0.));
#7415=DIRECTION('',(0.,1.,0.));
#7416=DIRECTION('center_axis',(0.,1.,0.));
#7417=DIRECTION('ref_axis',(1.,0.,0.));
#7418=DIRECTION('center_axis',(0.,-1.,0.));
#7419=DIRECTION('ref_axis',(1.,0.,0.));
#7420=DIRECTION('',(-0.707106781186548,0.707106781186547,-8.65956056235494E-17));
#7421=DIRECTION('center_axis',(0.,-1.,0.));
#7422=DIRECTION('ref_axis',(0.,0.,-1.));
#7423=DIRECTION('axis',(0.,0.,1.));
#7424=DIRECTION('refdir',(1.,0.,0.));
#7425=DIRECTION('center_axis',(0.,1.,0.));
#7426=DIRECTION('ref_axis',(1.,0.,0.));
#7427=DIRECTION('center_axis',(0.,-1.,0.));
#7428=DIRECTION('ref_axis',(1.,0.,0.));
#7429=DIRECTION('',(0.,-1.,0.));
#7430=DIRECTION('center_axis',(0.,-1.,0.));
#7431=DIRECTION('ref_axis',(1.,0.,0.));
#7432=DIRECTION('center_axis',(0.,1.,0.));
#7433=DIRECTION('ref_axis',(1.,0.,0.));
#7434=DIRECTION('center_axis',(0.,1.,0.));
#7435=DIRECTION('ref_axis',(1.,0.,0.));
#7436=DIRECTION('',(0.,-1.,0.));
#7437=DIRECTION('center_axis',(0.,1.,0.));
#7438=DIRECTION('ref_axis',(1.,0.,0.));
#7439=DIRECTION('center_axis',(0.,1.,0.));
#7440=DIRECTION('ref_axis',(1.,0.,0.));
#7441=DIRECTION('center_axis',(0.,1.,0.));
#7442=DIRECTION('ref_axis',(1.,0.,0.));
#7443=DIRECTION('axis',(0.,0.,1.));
#7444=DIRECTION('refdir',(1.,0.,0.));
#7445=DIRECTION('center_axis',(-1.,0.,0.));
#7446=DIRECTION('ref_axis',(0.,0.,1.));
#7447=DIRECTION('center_axis',(0.,-1.,1.38777878078145E-16));
#7448=DIRECTION('ref_axis',(0.,-1.38777878078145E-16,-1.));
#7449=DIRECTION('center_axis',(1.,0.,0.));
#7450=DIRECTION('ref_axis',(0.,0.,1.));
#7451=DIRECTION('center_axis',(0.,1.,0.));
#7452=DIRECTION('ref_axis',(1.,0.,0.));
#7453=DIRECTION('center_axis',(0.,-1.,0.));
#7454=DIRECTION('ref_axis',(1.,0.,0.));
#7455=DIRECTION('',(0.,0.,1.));
#7456=DIRECTION('center_axis',(1.,0.,0.));
#7457=DIRECTION('ref_axis',(0.,0.,1.));
#7458=DIRECTION('',(0.,-1.,0.));
#7459=DIRECTION('',(0.,0.,1.));
#7460=DIRECTION('',(0.,-1.,0.));
#7461=DIRECTION('center_axis',(0.,-1.,0.));
#7462=DIRECTION('ref_axis',(1.,0.,0.));
#7463=DIRECTION('center_axis',(0.,-1.,0.));
#7464=DIRECTION('ref_axis',(1.,0.,0.));
#7465=DIRECTION('',(0.,1.,0.));
#7466=DIRECTION('center_axis',(0.,-1.,0.));
#7467=DIRECTION('ref_axis',(1.,0.,0.));
#7468=DIRECTION('center_axis',(0.,1.,0.));
#7469=DIRECTION('ref_axis',(1.,0.,0.));
#7470=DIRECTION('',(0.,0.,1.));
#7471=DIRECTION('',(1.,0.,0.));
#7472=DIRECTION('',(0.,0.,1.));
#7473=DIRECTION('',(1.,0.,0.));
#7474=DIRECTION('',(0.,0.,1.));
#7475=DIRECTION('',(1.,0.,0.));
#7476=DIRECTION('',(0.,0.,1.));
#7477=DIRECTION('',(1.,0.,0.));
#7478=DIRECTION('',(0.,0.,1.));
#7479=DIRECTION('',(1.,0.,0.));
#7480=DIRECTION('',(0.,-1.,2.22044604925031E-16));
#7481=DIRECTION('',(1.,0.,0.));
#7482=DIRECTION('',(0.,0.,1.));
#7483=DIRECTION('',(2.22044604925031E-16,1.,0.));
#7484=DIRECTION('',(0.,0.,1.));
#7485=DIRECTION('',(2.22044604925031E-16,-1.,0.));
#7486=DIRECTION('',(0.,0.,1.));
#7487=DIRECTION('',(2.22044604925031E-16,-1.,0.));
#7488=DIRECTION('',(0.,0.,1.));
#7489=DIRECTION('',(2.22044604925031E-16,-1.,0.));
#7490=DIRECTION('',(0.,0.,1.));
#7491=DIRECTION('',(1.,0.,0.));
#7492=DIRECTION('',(0.,0.,1.));
#7493=DIRECTION('',(1.,0.,0.));
#7494=DIRECTION('',(0.,0.,1.));
#7495=DIRECTION('',(1.,0.,0.));
#7496=CARTESIAN_POINT('',(0.,0.,0.));
#7497=CARTESIAN_POINT('',(0.,0.,0.));
#7498=CARTESIAN_POINT('',(0.,0.,0.));
#7499=CARTESIAN_POINT('Origin',(-1.2,0.6,1.9));
#7500=CARTESIAN_POINT('',(-1.41,0.6,2.));
#7501=CARTESIAN_POINT('Origin',(-1.2,0.6,2.));
#7502=CARTESIAN_POINT('',(-1.41,0.6,3.1));
#7503=CARTESIAN_POINT('',(-1.41,0.6,1.9));
#7504=CARTESIAN_POINT('Origin',(-1.2,0.6,3.1));
#7505=CARTESIAN_POINT('Origin',(-1.2,0.6,3.1));
#7506=CARTESIAN_POINT('Origin',(1.2,0.6,1.9));
#7507=CARTESIAN_POINT('',(0.99,0.6,2.));
#7508=CARTESIAN_POINT('Origin',(1.2,0.6,2.));
#7509=CARTESIAN_POINT('',(0.99,0.6,3.1));
#7510=CARTESIAN_POINT('',(0.99,0.6,1.9));
#7511=CARTESIAN_POINT('Origin',(1.2,0.6,3.1));
#7512=CARTESIAN_POINT('Origin',(1.2,0.6,3.1));
#7513=CARTESIAN_POINT('Origin',(0.,0.7,5.4));
#7514=CARTESIAN_POINT('',(0.173205080756888,0.7,5.3));
#7515=CARTESIAN_POINT('',(-0.173205080756888,0.7,5.3));
#7516=CARTESIAN_POINT('',(0.,0.7,5.3));
#7517=CARTESIAN_POINT('Origin',(0.,0.7,5.4));
#7518=CARTESIAN_POINT('Origin',(0.,0.7,5.4));
#7519=CARTESIAN_POINT('',(0.173205080756888,0.7,5.5));
#7520=CARTESIAN_POINT('',(0.173205080756888,0.7,5.3));
#7521=CARTESIAN_POINT('Origin',(0.,0.7,5.4));
#7522=CARTESIAN_POINT('Origin',(0.,0.7,5.4));
#7523=CARTESIAN_POINT('',(0.2,0.8,5.4));
#7524=CARTESIAN_POINT('Origin',(0.,0.8,5.4));
#7525=CARTESIAN_POINT('Origin',(0.,0.8,5.4));
#7526=CARTESIAN_POINT('Origin',(0.,0.7,5.4));
#7527=CARTESIAN_POINT('',(-0.173205080756888,0.9,5.3));
#7528=CARTESIAN_POINT('',(-0.173205080756888,0.7,5.3));
#7529=CARTESIAN_POINT('',(0.173205080756888,0.9,5.3));
#7530=CARTESIAN_POINT('',(0.173205080756888,0.7,5.3));
#7531=CARTESIAN_POINT('Origin',(0.,0.8,5.4));
#7532=CARTESIAN_POINT('',(-0.2,0.8,5.4));
#7533=CARTESIAN_POINT('Origin',(0.,0.8,5.4));
#7534=CARTESIAN_POINT('',(-0.2,1.2,5.4));
#7535=CARTESIAN_POINT('',(-0.2,0.7,5.4));
#7536=CARTESIAN_POINT('',(-0.181811868577262,1.2,5.48333333333333));
#7537=CARTESIAN_POINT('Origin',(0.,1.2,5.4));
#7538=CARTESIAN_POINT('',(-0.181811868577262,1.5,5.48333333333333));
#7539=CARTESIAN_POINT('',(-0.181811868577262,0.7,5.48333333333333));
#7540=CARTESIAN_POINT('',(0.181811868577262,1.5,5.48333333333333));
#7541=CARTESIAN_POINT('Origin',(0.,1.5,5.4));
#7542=CARTESIAN_POINT('',(0.181811868577262,1.2,5.48333333333333));
#7543=CARTESIAN_POINT('',(0.181811868577262,0.7,5.48333333333333));
#7544=CARTESIAN_POINT('Origin',(0.,1.2,5.4));
#7545=CARTESIAN_POINT('Origin',(0.,0.8,5.4));
#7546=CARTESIAN_POINT('Origin',(0.,0.7,5.4));
#7547=CARTESIAN_POINT('',(-0.173205080756888,0.7,5.5));
#7548=CARTESIAN_POINT('Origin',(0.,0.8,5.4));
#7549=CARTESIAN_POINT('Origin',(0.,0.7,5.4));
#7550=CARTESIAN_POINT('Origin',(0.,0.8,5.4));
#7551=CARTESIAN_POINT('Origin',(0.,1.5,5.4));
#7552=CARTESIAN_POINT('Origin',(0.,1.5,4.5));
#7553=CARTESIAN_POINT('Origin',(0.,0.7,5.4));
#7554=CARTESIAN_POINT('',(-0.173205080756888,0.7,5.3));
#7555=CARTESIAN_POINT('Origin',(0.,0.8,5.3));
#7556=CARTESIAN_POINT('Origin',(0.,0.8,5.3));
#7557=CARTESIAN_POINT('Origin',(0.,0.8,5.3));
#7558=CARTESIAN_POINT('Origin',(0.,0.8,5.3));
#7559=CARTESIAN_POINT('Origin',(0.,0.8,5.3));
#7560=CARTESIAN_POINT('Origin',(0.,0.8,5.3));
#7561=CARTESIAN_POINT('',(-0.2,0.8,5.8));
#7562=CARTESIAN_POINT('',(-0.2,0.8,5.3));
#7563=CARTESIAN_POINT('Origin',(0.,0.8,5.8));
#7564=CARTESIAN_POINT('Origin',(0.,0.8,5.3));
#7565=CARTESIAN_POINT('Origin',(0.,0.8,5.3));
#7566=CARTESIAN_POINT('Origin',(0.,1.2,4.5));
#7567=CARTESIAN_POINT('',(-1.,1.2,4.5));
#7568=CARTESIAN_POINT('Origin',(0.,1.2,4.5));
#7569=CARTESIAN_POINT('',(-1.,1.7,4.5));
#7570=CARTESIAN_POINT('',(-1.,1.2,4.5));
#7571=CARTESIAN_POINT('Origin',(0.,1.7,4.5));
#7572=CARTESIAN_POINT('Origin',(0.,1.2,4.5));
#7573=CARTESIAN_POINT('Origin',(0.,0.8,5.3));
#7574=CARTESIAN_POINT('Origin',(0.,0.8,5.8));
#7575=CARTESIAN_POINT('',(-0.685,0.8,5.8));
#7576=CARTESIAN_POINT('Origin',(0.,0.8,5.8));
#7577=CARTESIAN_POINT('',(-0.685,0.8,7.));
#7578=CARTESIAN_POINT('',(-0.685,0.8,5.8));
#7579=CARTESIAN_POINT('Origin',(0.,0.8,7.));
#7580=CARTESIAN_POINT('Origin',(0.,0.8,5.8));
#7581=CARTESIAN_POINT('Origin',(2.,-0.1,2.5));
#7582=CARTESIAN_POINT('',(1.725,0.,2.5));
#7583=CARTESIAN_POINT('Origin',(2.,0.,2.5));
#7584=CARTESIAN_POINT('',(1.725,1.7,2.5));
#7585=CARTESIAN_POINT('',(1.725,-0.1,2.5));
#7586=CARTESIAN_POINT('Origin',(2.,1.7,2.5));
#7587=CARTESIAN_POINT('Origin',(-2.,-0.1,6.5));
#7588=CARTESIAN_POINT('',(-2.275,0.,6.5));
#7589=CARTESIAN_POINT('Origin',(-2.,0.,6.5));
#7590=CARTESIAN_POINT('',(-2.275,1.7,6.5));
#7591=CARTESIAN_POINT('',(-2.275,-0.1,6.5));
#7592=CARTESIAN_POINT('Origin',(-2.,1.7,6.5));
#7593=CARTESIAN_POINT('Origin',(-2.,-0.1,2.5));
#7594=CARTESIAN_POINT('',(-2.275,0.,2.5));
#7595=CARTESIAN_POINT('Origin',(-2.,0.,2.5));
#7596=CARTESIAN_POINT('',(-2.275,1.7,2.5));
#7597=CARTESIAN_POINT('',(-2.275,-0.1,2.5));
#7598=CARTESIAN_POINT('Origin',(-2.,1.7,2.5));
#7599=CARTESIAN_POINT('Origin',(2.,-0.1,6.5));
#7600=CARTESIAN_POINT('',(1.725,0.,6.5));
#7601=CARTESIAN_POINT('Origin',(2.,0.,6.5));
#7602=CARTESIAN_POINT('',(1.725,1.7,6.5));
#7603=CARTESIAN_POINT('',(1.725,-0.1,6.5));
#7604=CARTESIAN_POINT('Origin',(2.,1.7,6.5));
#7605=CARTESIAN_POINT('Origin',(0.,-0.1,4.5));
#7606=CARTESIAN_POINT('',(-0.6,0.,4.5));
#7607=CARTESIAN_POINT('Origin',(0.,0.,4.5));
#7608=CARTESIAN_POINT('',(-0.6,1.2,4.5));
#7609=CARTESIAN_POINT('',(-0.6,-0.1,4.5));
#7610=CARTESIAN_POINT('Origin',(0.,1.2,4.5));
#7611=CARTESIAN_POINT('Origin',(0.,1.2,4.5));
#7612=CARTESIAN_POINT('Origin',(2.5,1.7,2.));
#7613=CARTESIAN_POINT('',(2.5,1.7,2.));
#7614=CARTESIAN_POINT('',(-2.5,1.7,2.));
#7615=CARTESIAN_POINT('',(2.5,1.7,2.));
#7616=CARTESIAN_POINT('',(-2.5,1.7,7.));
#7617=CARTESIAN_POINT('',(-2.5,1.7,2.));
#7618=CARTESIAN_POINT('',(2.5,1.7,7.));
#7619=CARTESIAN_POINT('',(2.5,1.7,7.));
#7620=CARTESIAN_POINT('',(2.5,1.7,2.));
#7621=CARTESIAN_POINT('Origin',(2.5,0.,2.));
#7622=CARTESIAN_POINT('',(2.5,0.,2.));
#7623=CARTESIAN_POINT('',(2.5,0.,2.));
#7624=CARTESIAN_POINT('',(2.5,0.,7.));
#7625=CARTESIAN_POINT('',(2.5,0.,7.));
#7626=CARTESIAN_POINT('',(2.5,0.,2.));
#7627=CARTESIAN_POINT('Origin',(-2.5,0.,2.));
#7628=CARTESIAN_POINT('',(-2.5,0.,2.));
#7629=CARTESIAN_POINT('',(-2.5,0.,2.));
#7630=CARTESIAN_POINT('',(-2.5,0.,7.));
#7631=CARTESIAN_POINT('',(-2.5,0.,7.));
#7632=CARTESIAN_POINT('',(-2.5,0.,2.));
#7633=CARTESIAN_POINT('Origin',(-2.5,1.7,2.));
#7634=CARTESIAN_POINT('',(-2.5,1.7,2.));
#7635=CARTESIAN_POINT('',(-2.5,1.7,7.));
#7636=CARTESIAN_POINT('Origin',(0.,0.85,7.));
#7637=CARTESIAN_POINT('Origin',(0.,0.85,2.));
#7638=CARTESIAN_POINT('',(0.,0.,0.));
#7639=CARTESIAN_POINT('Origin',(0.35,0.8,8.5));
#7640=CARTESIAN_POINT('',(0.35,0.8,9.015));
#7641=CARTESIAN_POINT('Origin',(0.35,0.8,8.5));
#7642=CARTESIAN_POINT('',(1.,0.8,9.015));
#7643=CARTESIAN_POINT('',(0.35,0.8,9.015));
#7644=CARTESIAN_POINT('Origin',(1.,0.8,8.5));
#7645=CARTESIAN_POINT('Origin',(0.35,0.8,8.5));
#7646=CARTESIAN_POINT('',(0.35,0.606350832689629,8.9));
#7647=CARTESIAN_POINT('',(0.35,0.606350832689629,8.2));
#7648=CARTESIAN_POINT('',(0.35,0.606350832689629,8.2));
#7649=CARTESIAN_POINT('',(0.35,0.993649167310371,8.9));
#7650=CARTESIAN_POINT('',(0.35,0.8,8.9));
#7651=CARTESIAN_POINT('',(0.35,0.993649167310371,8.2));
#7652=CARTESIAN_POINT('',(0.35,0.993649167310371,8.2));
#7653=CARTESIAN_POINT('',(0.35,0.8,8.2));
#7654=CARTESIAN_POINT('Origin',(0.,0.8,8.9));
#7655=CARTESIAN_POINT('Origin',(0.,0.8,8.9));
#7656=CARTESIAN_POINT('',(-0.25,0.8,8.9));
#7657=CARTESIAN_POINT('Origin',(0.,0.8,8.9));
#7658=CARTESIAN_POINT('Origin',(0.,0.8,8.2));
#7659=CARTESIAN_POINT('Origin',(0.,0.8,8.2));
#7660=CARTESIAN_POINT('Origin',(0.,0.8,9.2));
#7661=CARTESIAN_POINT('',(-0.49,0.8,9.2));
#7662=CARTESIAN_POINT('Origin',(0.,0.8,9.2));
#7663=CARTESIAN_POINT('',(-0.49,0.8,9.4));
#7664=CARTESIAN_POINT('',(-0.49,0.8,9.2));
#7665=CARTESIAN_POINT('Origin',(0.,0.8,9.4));
#7666=CARTESIAN_POINT('Origin',(0.,0.8,9.4));
#7667=CARTESIAN_POINT('',(-0.25,0.8,9.4));
#7668=CARTESIAN_POINT('Origin',(0.,0.8,9.4));
#7669=CARTESIAN_POINT('Origin',(0.,0.8,9.2));
#7670=CARTESIAN_POINT('',(-0.25,0.8,9.2));
#7671=CARTESIAN_POINT('Origin',(0.,0.8,9.2));
#7672=CARTESIAN_POINT('Origin',(0.,0.8,8.8));
#7673=CARTESIAN_POINT('',(-0.25,0.8,8.8));
#7674=CARTESIAN_POINT('Origin',(0.,0.8,8.8));
#7675=CARTESIAN_POINT('',(-0.25,0.8,9.5));
#7676=CARTESIAN_POINT('',(-0.25,0.8,8.8));
#7677=CARTESIAN_POINT('Origin',(0.,0.8,9.5));
#7678=CARTESIAN_POINT('Origin',(0.,0.8,8.2));
#7679=CARTESIAN_POINT('',(-0.2,0.8,8.2));
#7680=CARTESIAN_POINT('Origin',(0.,0.8,8.2));
#7681=CARTESIAN_POINT('Origin',(0.,0.8,7.5));
#7682=CARTESIAN_POINT('',(-1.,0.782050807568877,7.5));
#7683=CARTESIAN_POINT('',(-0.505181485540923,-0.0749999999999997,7.5));
#7684=CARTESIAN_POINT('',(-1.01036297108185,0.8,7.5));
#7685=CARTESIAN_POINT('',(0.505181485540923,-0.075,7.5));
#7686=CARTESIAN_POINT('',(-0.505181485540923,-0.0749999999999997,7.5));
#7687=CARTESIAN_POINT('',(1.,0.782050807568877,7.5));
#7688=CARTESIAN_POINT('',(0.505181485540923,-0.075,7.5));
#7689=CARTESIAN_POINT('',(1.,-0.2,7.5));
#7690=CARTESIAN_POINT('',(1.,-0.2,7.5));
#7691=CARTESIAN_POINT('',(-1.,-0.2,7.5));
#7692=CARTESIAN_POINT('',(-1.,-0.2,7.5));
#7693=CARTESIAN_POINT('',(-1.,1.8,7.5));
#7694=CARTESIAN_POINT('Origin',(1.,1.8,7.5));
#7695=CARTESIAN_POINT('',(1.,1.8,7.5));
#7696=CARTESIAN_POINT('',(-1.,1.8,7.5));
#7697=CARTESIAN_POINT('',(1.,1.8,7.5));
#7698=CARTESIAN_POINT('',(-1.,1.8,9.5));
#7699=CARTESIAN_POINT('',(-1.,1.8,7.5));
#7700=CARTESIAN_POINT('',(1.,1.8,9.5));
#7701=CARTESIAN_POINT('',(1.,1.8,9.5));
#7702=CARTESIAN_POINT('',(1.,1.8,7.5));
#7703=CARTESIAN_POINT('Origin',(1.,-0.2,7.5));
#7704=CARTESIAN_POINT('',(1.,0.817949192431123,7.5));
#7705=CARTESIAN_POINT('',(1.,0.3,7.5));
#7706=CARTESIAN_POINT('',(1.,-0.2,7.5));
#7707=CARTESIAN_POINT('',(1.,-0.2,9.5));
#7708=CARTESIAN_POINT('',(1.,-0.2,9.5));
#7709=CARTESIAN_POINT('',(1.,-0.2,7.5));
#7710=CARTESIAN_POINT('Origin',(-1.,-0.2,7.5));
#7711=CARTESIAN_POINT('',(-1.,-0.2,9.5));
#7712=CARTESIAN_POINT('',(-1.,-0.2,9.5));
#7713=CARTESIAN_POINT('',(-1.,-0.2,7.5));
#7714=CARTESIAN_POINT('Origin',(-1.,1.8,7.5));
#7715=CARTESIAN_POINT('',(-1.,0.817949192431123,7.5));
#7716=CARTESIAN_POINT('',(-1.,1.8,7.5));
#7717=CARTESIAN_POINT('',(-1.,1.3,7.5));
#7718=CARTESIAN_POINT('',(-1.,1.8,9.5));
#7719=CARTESIAN_POINT('Origin',(0.,0.8,9.5));
#7720=CARTESIAN_POINT('Origin',(0.,0.8,7.5));
#7721=CARTESIAN_POINT('',(-0.505181485540922,1.675,7.5));
#7722=CARTESIAN_POINT('',(-0.505181485540922,1.675,7.5));
#7723=CARTESIAN_POINT('',(0.505181485540923,1.675,7.5));
#7724=CARTESIAN_POINT('',(1.01036297108185,0.8,7.5));
#7725=CARTESIAN_POINT('',(0.505181485540923,1.675,7.5));
#7726=CARTESIAN_POINT('Origin',(0.,0.8,7.5));
#7727=CARTESIAN_POINT('',(1.01036297108185,0.8,7.5));
#7728=CARTESIAN_POINT('',(0.505181485540923,-0.075,7.5));
#7729=CARTESIAN_POINT('',(1.01036297108185,0.8,7.5));
#7730=CARTESIAN_POINT('Origin',(0.,0.8,7.));
#7731=CARTESIAN_POINT('',(0.505181485540923,-0.075,7.));
#7732=CARTESIAN_POINT('',(1.01036297108185,0.8,7.));
#7733=CARTESIAN_POINT('',(0.505181485540923,-0.075,7.));
#7734=CARTESIAN_POINT('',(-0.505181485540923,-0.0749999999999997,7.));
#7735=CARTESIAN_POINT('',(-0.505181485540923,-0.0749999999999997,7.));
#7736=CARTESIAN_POINT('',(-1.01036297108185,0.8,7.));
#7737=CARTESIAN_POINT('',(-1.01036297108185,0.8,7.));
#7738=CARTESIAN_POINT('',(-0.505181485540922,1.675,7.));
#7739=CARTESIAN_POINT('',(-0.505181485540922,1.675,7.));
#7740=CARTESIAN_POINT('',(0.505181485540923,1.675,7.));
#7741=CARTESIAN_POINT('',(0.505181485540923,1.675,7.));
#7742=CARTESIAN_POINT('',(1.01036297108185,0.8,7.));
#7743=CARTESIAN_POINT('',(-0.685,0.8,7.));
#7744=CARTESIAN_POINT('Origin',(0.,0.8,7.));
#7745=CARTESIAN_POINT('Origin',(-0.505181485540923,-0.0749999999999997,
7.));
#7746=CARTESIAN_POINT('',(0.505181485540923,-0.075,7.));
#7747=CARTESIAN_POINT('',(-0.505181485540923,-0.0749999999999997,7.));
#7748=CARTESIAN_POINT('Origin',(-1.01036297108185,0.8,7.));
#7749=CARTESIAN_POINT('',(-1.01036297108185,0.8,7.5));
#7750=CARTESIAN_POINT('',(-1.01036297108185,0.8,7.5));
#7751=CARTESIAN_POINT('',(-1.01036297108185,0.8,7.));
#7752=CARTESIAN_POINT('Origin',(-0.505181485540922,1.675,7.));
#7753=CARTESIAN_POINT('',(-0.505181485540922,1.675,7.5));
#7754=CARTESIAN_POINT('',(-0.505181485540922,1.675,7.));
#7755=CARTESIAN_POINT('Origin',(0.505181485540923,1.675,7.));
#7756=CARTESIAN_POINT('',(0.505181485540923,1.675,7.));
#7757=CARTESIAN_POINT('Origin',(1.01036297108185,0.8,7.));
#7758=CARTESIAN_POINT('',(1.01036297108185,0.8,7.));
#7759=CARTESIAN_POINT('Origin',(0.505181485540923,-0.075,7.));
#7760=CARTESIAN_POINT('Origin',(0.,0.8,7.5));
#7761=CARTESIAN_POINT('Origin',(0.,0.8,5.8));
#7762=CARTESIAN_POINT('',(-0.2,0.8,5.8));
#7763=CARTESIAN_POINT('',(-0.2,0.8,5.8));
#7764=CARTESIAN_POINT('Origin',(0.,0.8,5.8));
#7765=CARTESIAN_POINT('Origin',(0.,0.8,5.8));
#7766=CARTESIAN_POINT('',(-0.685,0.8,5.8));
#7767=CARTESIAN_POINT('',(-0.685,0.8,5.8));
#7768=CARTESIAN_POINT('Origin',(0.,0.8,5.8));
#7769=CARTESIAN_POINT('Origin',(0.,0.8,5.8));
#7770=CARTESIAN_POINT('',(0.,0.,0.));
#7771=CARTESIAN_POINT('Origin',(0.,0.8,8.15));
#7772=CARTESIAN_POINT('',(-0.2,0.8,8.25));
#7773=CARTESIAN_POINT('Origin',(0.,0.8,8.25));
#7774=CARTESIAN_POINT('',(0.,0.8,8.05));
#7775=CARTESIAN_POINT('',(-0.1,0.8,8.15));
#7776=CARTESIAN_POINT('Origin',(0.,0.8,8.4));
#7777=CARTESIAN_POINT('',(-0.3,0.8,8.55));
#7778=CARTESIAN_POINT('Origin',(0.,0.8,8.55));
#7779=CARTESIAN_POINT('',(-0.25,0.8,8.4));
#7780=CARTESIAN_POINT('Origin',(0.,0.8,9.425));
#7781=CARTESIAN_POINT('',(-0.3,0.8,10.3));
#7782=CARTESIAN_POINT('Origin',(0.,0.8,10.3));
#7783=CARTESIAN_POINT('',(-0.3,0.8,9.425));
#7784=CARTESIAN_POINT('Origin',(0.6,0.8,10.3));
#7785=CARTESIAN_POINT('',(-0.6,0.8,10.3));
#7786=CARTESIAN_POINT('Origin',(0.,0.8,10.3));
#7787=CARTESIAN_POINT('Origin',(0.,0.8,10.6));
#7788=CARTESIAN_POINT('',(-0.6,0.8,10.9));
#7789=CARTESIAN_POINT('Origin',(0.,0.8,10.9));
#7790=CARTESIAN_POINT('',(-0.6,0.8,10.6));
#7791=CARTESIAN_POINT('Origin',(0.,0.8,10.9));
#7792=CARTESIAN_POINT('',(0.,0.,0.));
#7793=CARTESIAN_POINT('Origin',(-1.2,12.,1.9));
#7794=CARTESIAN_POINT('',(-1.41,12.,2.));
#7795=CARTESIAN_POINT('Origin',(-1.2,12.,2.));
#7796=CARTESIAN_POINT('',(-1.41,12.,3.1));
#7797=CARTESIAN_POINT('',(-1.41,12.,1.9));
#7798=CARTESIAN_POINT('Origin',(-1.2,12.,3.1));
#7799=CARTESIAN_POINT('Origin',(-1.2,12.,3.1));
#7800=CARTESIAN_POINT('Origin',(1.2,12.,1.9));
#7801=CARTESIAN_POINT('',(0.99,12.,2.));
#7802=CARTESIAN_POINT('Origin',(1.2,12.,2.));
#7803=CARTESIAN_POINT('',(0.99,12.,3.1));
#7804=CARTESIAN_POINT('',(0.99,12.,1.9));
#7805=CARTESIAN_POINT('Origin',(1.2,12.,3.1));
#7806=CARTESIAN_POINT('Origin',(1.2,12.,3.1));
#7807=CARTESIAN_POINT('Origin',(0.,11.9,5.4));
#7808=CARTESIAN_POINT('',(-0.173205080756887,11.9,5.3));
#7809=CARTESIAN_POINT('',(0.173205080756887,11.9,5.3));
#7810=CARTESIAN_POINT('',(0.,11.9,5.3));
#7811=CARTESIAN_POINT('Origin',(0.,11.9,5.4));
#7812=CARTESIAN_POINT('Origin',(0.,11.9,5.4));
#7813=CARTESIAN_POINT('',(0.173205080756887,11.9,5.5));
#7814=CARTESIAN_POINT('',(0.173205080756887,11.9,5.3));
#7815=CARTESIAN_POINT('Origin',(0.,11.9,5.4));
#7816=CARTESIAN_POINT('Origin',(0.,11.9,5.4));
#7817=CARTESIAN_POINT('',(-0.173205080756887,11.9,5.5));
#7818=CARTESIAN_POINT('',(-0.173205080756887,11.9,5.3));
#7819=CARTESIAN_POINT('Origin',(0.,11.9,5.4));
#7820=CARTESIAN_POINT('Origin',(0.,11.1,5.4));
#7821=CARTESIAN_POINT('',(0.181811868577262,11.1,5.48333333333333));
#7822=CARTESIAN_POINT('',(0.181811868577262,11.4,5.48333333333333));
#7823=CARTESIAN_POINT('',(0.181811868577262,11.1,5.48333333333333));
#7824=CARTESIAN_POINT('',(-0.181811868577262,11.1,5.48333333333333));
#7825=CARTESIAN_POINT('Origin',(0.,11.1,5.4));
#7826=CARTESIAN_POINT('',(-0.181811868577262,11.4,5.48333333333333));
#7827=CARTESIAN_POINT('',(-0.181811868577262,11.1,5.48333333333333));
#7828=CARTESIAN_POINT('',(-0.2,11.4,5.4));
#7829=CARTESIAN_POINT('Origin',(0.,11.4,5.4));
#7830=CARTESIAN_POINT('',(-0.2,11.8,5.4));
#7831=CARTESIAN_POINT('',(-0.2,11.1,5.4));
#7832=CARTESIAN_POINT('',(0.2,11.8,5.4));
#7833=CARTESIAN_POINT('Origin',(0.,11.8,5.4));
#7834=CARTESIAN_POINT('',(0.173205080756888,11.7,5.3));
#7835=CARTESIAN_POINT('Origin',(0.,11.8,5.4));
#7836=CARTESIAN_POINT('',(0.173205080756888,11.1,5.3));
#7837=CARTESIAN_POINT('',(-0.173205080756888,11.7,5.3));
#7838=CARTESIAN_POINT('',(-0.173205080756888,11.1,5.3));
#7839=CARTESIAN_POINT('Origin',(0.,11.8,5.4));
#7840=CARTESIAN_POINT('Origin',(0.,11.4,5.4));
#7841=CARTESIAN_POINT('Origin',(0.,11.1,5.4));
#7842=CARTESIAN_POINT('Origin',(0.,11.8,5.4));
#7843=CARTESIAN_POINT('Origin',(0.,11.8,5.4));
#7844=CARTESIAN_POINT('Origin',(0.,11.1,5.4));
#7845=CARTESIAN_POINT('Origin',(0.,11.8,5.4));
#7846=CARTESIAN_POINT('Origin',(0.,11.8,5.4));
#7847=CARTESIAN_POINT('Origin',(0.,11.1,5.4));
#7848=CARTESIAN_POINT('Origin',(0.,11.1,4.5));
#7849=CARTESIAN_POINT('Origin',(0.,11.8,5.3));
#7850=CARTESIAN_POINT('Origin',(0.,11.8,5.3));
#7851=CARTESIAN_POINT('Origin',(0.,11.8,5.3));
#7852=CARTESIAN_POINT('Origin',(0.,11.8,5.3));
#7853=CARTESIAN_POINT('Origin',(0.,11.8,5.3));
#7854=CARTESIAN_POINT('Origin',(0.,11.8,5.3));
#7855=CARTESIAN_POINT('Origin',(0.,11.8,5.3));
#7856=CARTESIAN_POINT('Origin',(0.,11.8,5.3));
#7857=CARTESIAN_POINT('Origin',(0.,11.8,5.3));
#7858=CARTESIAN_POINT('',(-0.2,11.8,5.8));
#7859=CARTESIAN_POINT('',(-0.2,11.8,5.3));
#7860=CARTESIAN_POINT('Origin',(0.,11.8,5.8));
#7861=CARTESIAN_POINT('Origin',(0.,11.4,4.5));
#7862=CARTESIAN_POINT('',(-1.,11.4,4.5));
#7863=CARTESIAN_POINT('Origin',(0.,11.4,4.5));
#7864=CARTESIAN_POINT('Origin',(0.,11.4,4.5));
#7865=CARTESIAN_POINT('Origin',(0.,11.8,5.8));
#7866=CARTESIAN_POINT('',(-0.685,11.8,5.8));
#7867=CARTESIAN_POINT('Origin',(0.,11.8,5.8));
#7868=CARTESIAN_POINT('',(-0.685,11.8,7.));
#7869=CARTESIAN_POINT('',(-0.685,11.8,5.8));
#7870=CARTESIAN_POINT('Origin',(0.,11.8,7.));
#7871=CARTESIAN_POINT('Origin',(0.,11.8,5.8));
#7872=CARTESIAN_POINT('Origin',(2.,10.8,2.5));
#7873=CARTESIAN_POINT('',(1.725,10.9,2.5));
#7874=CARTESIAN_POINT('Origin',(2.,10.9,2.5));
#7875=CARTESIAN_POINT('',(1.725,12.6,2.5));
#7876=CARTESIAN_POINT('',(1.725,10.8,2.5));
#7877=CARTESIAN_POINT('Origin',(2.,12.6,2.5));
#7878=CARTESIAN_POINT('Origin',(-2.,10.8,6.5));
#7879=CARTESIAN_POINT('',(-2.275,10.9,6.5));
#7880=CARTESIAN_POINT('Origin',(-2.,10.9,6.5));
#7881=CARTESIAN_POINT('',(-2.275,12.6,6.5));
#7882=CARTESIAN_POINT('',(-2.275,10.8,6.5));
#7883=CARTESIAN_POINT('Origin',(-2.,12.6,6.5));
#7884=CARTESIAN_POINT('Origin',(-2.,10.8,2.5));
#7885=CARTESIAN_POINT('',(-2.275,10.9,2.5));
#7886=CARTESIAN_POINT('Origin',(-2.,10.9,2.5));
#7887=CARTESIAN_POINT('',(-2.275,12.6,2.5));
#7888=CARTESIAN_POINT('',(-2.275,10.8,2.5));
#7889=CARTESIAN_POINT('Origin',(-2.,12.6,2.5));
#7890=CARTESIAN_POINT('Origin',(2.,10.8,6.5));
#7891=CARTESIAN_POINT('',(1.725,10.9,6.5));
#7892=CARTESIAN_POINT('Origin',(2.,10.9,6.5));
#7893=CARTESIAN_POINT('',(1.725,12.6,6.5));
#7894=CARTESIAN_POINT('',(1.725,10.8,6.5));
#7895=CARTESIAN_POINT('Origin',(2.,12.6,6.5));
#7896=CARTESIAN_POINT('Origin',(0.,10.8,4.5));
#7897=CARTESIAN_POINT('',(-1.,10.9,4.5));
#7898=CARTESIAN_POINT('Origin',(0.,10.9,4.5));
#7899=CARTESIAN_POINT('',(-1.,10.8,4.5));
#7900=CARTESIAN_POINT('Origin',(2.5,12.6,2.));
#7901=CARTESIAN_POINT('',(2.5,12.6,2.));
#7902=CARTESIAN_POINT('',(-2.5,12.6,2.));
#7903=CARTESIAN_POINT('',(2.5,12.6,2.));
#7904=CARTESIAN_POINT('',(-2.5,12.6,7.));
#7905=CARTESIAN_POINT('',(-2.5,12.6,2.));
#7906=CARTESIAN_POINT('',(2.5,12.6,7.));
#7907=CARTESIAN_POINT('',(2.5,12.6,7.));
#7908=CARTESIAN_POINT('',(2.5,12.6,2.));
#7909=CARTESIAN_POINT('Origin',(2.5,10.9,2.));
#7910=CARTESIAN_POINT('',(2.5,10.9,2.));
#7911=CARTESIAN_POINT('',(2.5,10.9,2.));
#7912=CARTESIAN_POINT('',(2.5,10.9,7.));
#7913=CARTESIAN_POINT('',(2.5,10.9,7.));
#7914=CARTESIAN_POINT('',(2.5,10.9,2.));
#7915=CARTESIAN_POINT('Origin',(-2.5,10.9,2.));
#7916=CARTESIAN_POINT('',(-2.5,10.9,2.));
#7917=CARTESIAN_POINT('',(-2.5,10.9,2.));
#7918=CARTESIAN_POINT('',(-2.5,10.9,7.));
#7919=CARTESIAN_POINT('',(-2.5,10.9,7.));
#7920=CARTESIAN_POINT('',(-2.5,10.9,2.));
#7921=CARTESIAN_POINT('Origin',(-2.5,12.6,2.));
#7922=CARTESIAN_POINT('',(-2.5,12.6,2.));
#7923=CARTESIAN_POINT('',(-2.5,12.6,7.));
#7924=CARTESIAN_POINT('Origin',(0.,11.75,7.));
#7925=CARTESIAN_POINT('Origin',(0.,11.75,2.));
#7926=CARTESIAN_POINT('',(0.,0.,0.));
#7927=CARTESIAN_POINT('Origin',(0.35,11.8,8.5));
#7928=CARTESIAN_POINT('',(0.35,11.8,9.015));
#7929=CARTESIAN_POINT('Origin',(0.35,11.8,8.5));
#7930=CARTESIAN_POINT('',(1.,11.8,9.015));
#7931=CARTESIAN_POINT('',(0.35,11.8,9.015));
#7932=CARTESIAN_POINT('Origin',(1.,11.8,8.5));
#7933=CARTESIAN_POINT('Origin',(0.35,11.8,8.5));
#7934=CARTESIAN_POINT('',(0.35,11.6063508326896,8.9));
#7935=CARTESIAN_POINT('',(0.35,11.6063508326896,8.2));
#7936=CARTESIAN_POINT('',(0.35,11.6063508326896,8.2));
#7937=CARTESIAN_POINT('',(0.35,11.9936491673104,8.9));
#7938=CARTESIAN_POINT('',(0.35,11.8,8.9));
#7939=CARTESIAN_POINT('',(0.35,11.9936491673104,8.2));
#7940=CARTESIAN_POINT('',(0.35,11.9936491673104,8.2));
#7941=CARTESIAN_POINT('',(0.35,11.8,8.2));
#7942=CARTESIAN_POINT('Origin',(0.,11.8,8.9));
#7943=CARTESIAN_POINT('Origin',(0.,11.8,8.9));
#7944=CARTESIAN_POINT('',(-0.25,11.8,8.9));
#7945=CARTESIAN_POINT('Origin',(0.,11.8,8.9));
#7946=CARTESIAN_POINT('Origin',(0.,11.8,8.2));
#7947=CARTESIAN_POINT('Origin',(0.,11.8,8.2));
#7948=CARTESIAN_POINT('Origin',(0.,11.8,9.2));
#7949=CARTESIAN_POINT('',(-0.49,11.8,9.2));
#7950=CARTESIAN_POINT('Origin',(0.,11.8,9.2));
#7951=CARTESIAN_POINT('',(-0.49,11.8,9.4));
#7952=CARTESIAN_POINT('',(-0.49,11.8,9.2));
#7953=CARTESIAN_POINT('Origin',(0.,11.8,9.4));
#7954=CARTESIAN_POINT('Origin',(0.,11.8,9.4));
#7955=CARTESIAN_POINT('',(-0.25,11.8,9.4));
#7956=CARTESIAN_POINT('Origin',(0.,11.8,9.4));
#7957=CARTESIAN_POINT('Origin',(0.,11.8,9.2));
#7958=CARTESIAN_POINT('',(-0.25,11.8,9.2));
#7959=CARTESIAN_POINT('Origin',(0.,11.8,9.2));
#7960=CARTESIAN_POINT('Origin',(0.,11.8,8.8));
#7961=CARTESIAN_POINT('',(-0.25,11.8,8.8));
#7962=CARTESIAN_POINT('Origin',(0.,11.8,8.8));
#7963=CARTESIAN_POINT('',(-0.25,11.8,9.5));
#7964=CARTESIAN_POINT('',(-0.25,11.8,8.8));
#7965=CARTESIAN_POINT('Origin',(0.,11.8,9.5));
#7966=CARTESIAN_POINT('Origin',(0.,11.8,8.2));
#7967=CARTESIAN_POINT('',(-0.2,11.8,8.2));
#7968=CARTESIAN_POINT('Origin',(0.,11.8,8.2));
#7969=CARTESIAN_POINT('Origin',(0.,11.8,7.5));
#7970=CARTESIAN_POINT('',(-1.,11.7820508075689,7.5));
#7971=CARTESIAN_POINT('',(-0.505181485540923,10.925,7.5));
#7972=CARTESIAN_POINT('',(-1.01036297108185,11.8,7.5));
#7973=CARTESIAN_POINT('',(0.505181485540923,10.925,7.5));
#7974=CARTESIAN_POINT('',(-0.505181485540923,10.925,7.5));
#7975=CARTESIAN_POINT('',(1.,11.7820508075689,7.5));
#7976=CARTESIAN_POINT('',(0.505181485540923,10.925,7.5));
#7977=CARTESIAN_POINT('',(1.,10.8,7.5));
#7978=CARTESIAN_POINT('',(1.,10.8,7.5));
#7979=CARTESIAN_POINT('',(-1.,10.8,7.5));
#7980=CARTESIAN_POINT('',(-1.,10.8,7.5));
#7981=CARTESIAN_POINT('',(-1.,12.8,7.5));
#7982=CARTESIAN_POINT('Origin',(1.,12.8,7.5));
#7983=CARTESIAN_POINT('',(1.,12.8,7.5));
#7984=CARTESIAN_POINT('',(-1.,12.8,7.5));
#7985=CARTESIAN_POINT('',(1.,12.8,7.5));
#7986=CARTESIAN_POINT('',(-1.,12.8,9.5));
#7987=CARTESIAN_POINT('',(-1.,12.8,7.5));
#7988=CARTESIAN_POINT('',(1.,12.8,9.5));
#7989=CARTESIAN_POINT('',(1.,12.8,9.5));
#7990=CARTESIAN_POINT('',(1.,12.8,7.5));
#7991=CARTESIAN_POINT('Origin',(1.,10.8,7.5));
#7992=CARTESIAN_POINT('',(1.,11.8179491924311,7.5));
#7993=CARTESIAN_POINT('',(1.,11.3,7.5));
#7994=CARTESIAN_POINT('',(1.,10.8,7.5));
#7995=CARTESIAN_POINT('',(1.,10.8,9.5));
#7996=CARTESIAN_POINT('',(1.,10.8,9.5));
#7997=CARTESIAN_POINT('',(1.,10.8,7.5));
#7998=CARTESIAN_POINT('Origin',(-1.,10.8,7.5));
#7999=CARTESIAN_POINT('',(-1.,10.8,9.5));
#8000=CARTESIAN_POINT('',(-1.,10.8,9.5));
#8001=CARTESIAN_POINT('',(-1.,10.8,7.5));
#8002=CARTESIAN_POINT('Origin',(-1.,12.8,7.5));
#8003=CARTESIAN_POINT('',(-1.,11.8179491924311,7.5));
#8004=CARTESIAN_POINT('',(-1.,12.8,7.5));
#8005=CARTESIAN_POINT('',(-1.,12.3,7.5));
#8006=CARTESIAN_POINT('',(-1.,12.8,9.5));
#8007=CARTESIAN_POINT('Origin',(0.,11.8,9.5));
#8008=CARTESIAN_POINT('Origin',(0.,11.8,7.5));
#8009=CARTESIAN_POINT('',(-0.505181485540922,12.675,7.5));
#8010=CARTESIAN_POINT('',(-0.505181485540922,12.675,7.5));
#8011=CARTESIAN_POINT('',(0.505181485540923,12.675,7.5));
#8012=CARTESIAN_POINT('',(1.01036297108185,11.8,7.5));
#8013=CARTESIAN_POINT('',(0.505181485540923,12.675,7.5));
#8014=CARTESIAN_POINT('Origin',(0.,11.8,7.5));
#8015=CARTESIAN_POINT('',(1.01036297108185,11.8,7.5));
#8016=CARTESIAN_POINT('',(0.505181485540923,10.925,7.5));
#8017=CARTESIAN_POINT('',(1.01036297108185,11.8,7.5));
#8018=CARTESIAN_POINT('Origin',(0.,11.8,7.));
#8019=CARTESIAN_POINT('',(0.505181485540923,10.925,7.));
#8020=CARTESIAN_POINT('',(1.01036297108185,11.8,7.));
#8021=CARTESIAN_POINT('',(0.505181485540923,10.925,7.));
#8022=CARTESIAN_POINT('',(-0.505181485540923,10.925,7.));
#8023=CARTESIAN_POINT('',(-0.505181485540923,10.925,7.));
#8024=CARTESIAN_POINT('',(-1.01036297108185,11.8,7.));
#8025=CARTESIAN_POINT('',(-1.01036297108185,11.8,7.));
#8026=CARTESIAN_POINT('',(-0.505181485540922,12.675,7.));
#8027=CARTESIAN_POINT('',(-0.505181485540922,12.675,7.));
#8028=CARTESIAN_POINT('',(0.505181485540923,12.675,7.));
#8029=CARTESIAN_POINT('',(0.505181485540923,12.675,7.));
#8030=CARTESIAN_POINT('',(1.01036297108185,11.8,7.));
#8031=CARTESIAN_POINT('',(-0.685,11.8,7.));
#8032=CARTESIAN_POINT('Origin',(0.,11.8,7.));
#8033=CARTESIAN_POINT('Origin',(-0.505181485540923,10.925,7.));
#8034=CARTESIAN_POINT('',(0.505181485540923,10.925,7.));
#8035=CARTESIAN_POINT('',(-0.505181485540923,10.925,7.));
#8036=CARTESIAN_POINT('Origin',(-1.01036297108185,11.8,7.));
#8037=CARTESIAN_POINT('',(-1.01036297108185,11.8,7.5));
#8038=CARTESIAN_POINT('',(-1.01036297108185,11.8,7.5));
#8039=CARTESIAN_POINT('',(-1.01036297108185,11.8,7.));
#8040=CARTESIAN_POINT('Origin',(-0.505181485540922,12.675,7.));
#8041=CARTESIAN_POINT('',(-0.505181485540922,12.675,7.5));
#8042=CARTESIAN_POINT('',(-0.505181485540922,12.675,7.));
#8043=CARTESIAN_POINT('Origin',(0.505181485540923,12.675,7.));
#8044=CARTESIAN_POINT('',(0.505181485540923,12.675,7.));
#8045=CARTESIAN_POINT('Origin',(1.01036297108185,11.8,7.));
#8046=CARTESIAN_POINT('',(1.01036297108185,11.8,7.));
#8047=CARTESIAN_POINT('Origin',(0.505181485540923,10.925,7.));
#8048=CARTESIAN_POINT('Origin',(0.,11.8,7.5));
#8049=CARTESIAN_POINT('Origin',(0.,11.8,5.8));
#8050=CARTESIAN_POINT('',(-0.2,11.8,5.8));
#8051=CARTESIAN_POINT('',(-0.2,11.8,5.8));
#8052=CARTESIAN_POINT('Origin',(0.,11.8,5.8));
#8053=CARTESIAN_POINT('Origin',(0.,11.8,5.8));
#8054=CARTESIAN_POINT('',(-0.685,11.8,5.8));
#8055=CARTESIAN_POINT('',(-0.685,11.8,5.8));
#8056=CARTESIAN_POINT('Origin',(0.,11.8,5.8));
#8057=CARTESIAN_POINT('Origin',(0.,11.8,5.8));
#8058=CARTESIAN_POINT('',(0.,0.,0.));
#8059=CARTESIAN_POINT('Origin',(0.,11.8,8.15));
#8060=CARTESIAN_POINT('',(-0.2,11.8,8.25));
#8061=CARTESIAN_POINT('Origin',(0.,11.8,8.25));
#8062=CARTESIAN_POINT('',(0.,11.8,8.05));
#8063=CARTESIAN_POINT('',(-0.1,11.8,8.15));
#8064=CARTESIAN_POINT('Origin',(0.,11.8,8.4));
#8065=CARTESIAN_POINT('',(-0.3,11.8,8.55));
#8066=CARTESIAN_POINT('Origin',(0.,11.8,8.55));
#8067=CARTESIAN_POINT('',(-0.25,11.8,8.4));
#8068=CARTESIAN_POINT('Origin',(0.,11.8,9.425));
#8069=CARTESIAN_POINT('',(-0.3,11.8,10.3));
#8070=CARTESIAN_POINT('Origin',(0.,11.8,10.3));
#8071=CARTESIAN_POINT('',(-0.3,11.8,9.425));
#8072=CARTESIAN_POINT('Origin',(0.6,11.8,10.3));
#8073=CARTESIAN_POINT('',(-0.6,11.8,10.3));
#8074=CARTESIAN_POINT('Origin',(0.,11.8,10.3));
#8075=CARTESIAN_POINT('Origin',(0.,11.8,10.6));
#8076=CARTESIAN_POINT('',(-0.6,11.8,10.9));
#8077=CARTESIAN_POINT('Origin',(0.,11.8,10.9));
#8078=CARTESIAN_POINT('',(-0.6,11.8,10.6));
#8079=CARTESIAN_POINT('Origin',(0.,11.8,10.9));
#8080=CARTESIAN_POINT('',(0.,0.,0.));
#8081=CARTESIAN_POINT('Origin',(0.,1.8,4.5));
#8082=CARTESIAN_POINT('',(-1.,10.8,4.5));
#8083=CARTESIAN_POINT('Origin',(0.,10.8,4.5));
#8084=CARTESIAN_POINT('',(-1.,1.8,4.5));
#8085=CARTESIAN_POINT('',(-1.,1.8,4.5));
#8086=CARTESIAN_POINT('Origin',(0.,1.8,4.5));
#8087=CARTESIAN_POINT('Origin',(0.,1.8,4.5));
#8088=CARTESIAN_POINT('',(-1.6,10.8,4.5));
#8089=CARTESIAN_POINT('Origin',(0.,10.8,4.5));
#8090=CARTESIAN_POINT('',(-1.6,1.8,4.5));
#8091=CARTESIAN_POINT('',(-1.6,1.8,4.5));
#8092=CARTESIAN_POINT('Origin',(0.,1.8,4.5));
#8093=CARTESIAN_POINT('Origin',(0.,10.8,4.5));
#8094=CARTESIAN_POINT('Origin',(0.,1.8,4.5));
#8095=CARTESIAN_POINT('',(0.,0.,0.));
#8096=CARTESIAN_POINT('Origin',(0.,1.7,4.5));
#8097=CARTESIAN_POINT('',(-1.,1.8,4.5));
#8098=CARTESIAN_POINT('Origin',(0.,1.8,4.5));
#8099=CARTESIAN_POINT('',(-1.,1.7,4.5));
#8100=CARTESIAN_POINT('',(-1.,1.7,4.5));
#8101=CARTESIAN_POINT('Origin',(0.,1.7,4.5));
#8102=CARTESIAN_POINT('Origin',(0.,1.7,4.5));
#8103=CARTESIAN_POINT('',(-1.6,1.8,4.5));
#8104=CARTESIAN_POINT('Origin',(0.,1.8,4.5));
#8105=CARTESIAN_POINT('',(-1.6,1.7,4.5));
#8106=CARTESIAN_POINT('',(-1.6,1.7,4.5));
#8107=CARTESIAN_POINT('Origin',(0.,1.7,4.5));
#8108=CARTESIAN_POINT('Origin',(0.,1.8,4.5));
#8109=CARTESIAN_POINT('Origin',(0.,1.7,4.5));
#8110=CARTESIAN_POINT('',(0.,0.,0.));
#8111=CARTESIAN_POINT('Origin',(0.,10.8,4.5));
#8112=CARTESIAN_POINT('',(-1.,10.9,4.5));
#8113=CARTESIAN_POINT('Origin',(0.,10.9,4.5));
#8114=CARTESIAN_POINT('',(-1.,10.8,4.5));
#8115=CARTESIAN_POINT('',(-1.,10.8,4.5));
#8116=CARTESIAN_POINT('Origin',(0.,10.8,4.5));
#8117=CARTESIAN_POINT('Origin',(0.,10.8,4.5));
#8118=CARTESIAN_POINT('',(-1.6,10.9,4.5));
#8119=CARTESIAN_POINT('Origin',(0.,10.9,4.5));
#8120=CARTESIAN_POINT('',(-1.6,10.8,4.5));
#8121=CARTESIAN_POINT('',(-1.6,10.8,4.5));
#8122=CARTESIAN_POINT('Origin',(0.,10.8,4.5));
#8123=CARTESIAN_POINT('Origin',(0.,10.9,4.5));
#8124=CARTESIAN_POINT('Origin',(0.,10.8,4.5));
#8125=CARTESIAN_POINT('',(0.,0.,0.));
#8126=CARTESIAN_POINT('Origin',(-2.9,0.9,-0.1));
#8127=CARTESIAN_POINT('',(-3.175,0.9,0.));
#8128=CARTESIAN_POINT('Origin',(-2.9,0.9,0.));
#8129=CARTESIAN_POINT('',(-3.175,0.9,2.));
#8130=CARTESIAN_POINT('',(-3.175,0.9,-0.1));
#8131=CARTESIAN_POINT('Origin',(-2.9,0.9,2.));
#8132=CARTESIAN_POINT('Origin',(2.9,0.9,-0.1));
#8133=CARTESIAN_POINT('',(2.625,0.9,0.));
#8134=CARTESIAN_POINT('Origin',(2.9,0.9,0.));
#8135=CARTESIAN_POINT('',(2.625,0.9,2.));
#8136=CARTESIAN_POINT('',(2.625,0.9,-0.1));
#8137=CARTESIAN_POINT('Origin',(2.9,0.9,2.));
#8138=CARTESIAN_POINT('Origin',(-1.2,0.6,-0.1));
#8139=CARTESIAN_POINT('',(-1.7,0.6,0.));
#8140=CARTESIAN_POINT('Origin',(-1.2,0.6,0.));
#8141=CARTESIAN_POINT('',(-1.7,0.6,0.8));
#8142=CARTESIAN_POINT('',(-1.7,0.6,-0.1));
#8143=CARTESIAN_POINT('Origin',(-1.2,0.6,0.8));
#8144=CARTESIAN_POINT('Origin',(-1.2,0.6,0.8));
#8145=CARTESIAN_POINT('',(-1.475,0.6,0.8));
#8146=CARTESIAN_POINT('Origin',(-1.2,0.6,0.8));
#8147=CARTESIAN_POINT('Origin',(1.2,0.6,-0.1));
#8148=CARTESIAN_POINT('',(0.7,0.6,0.));
#8149=CARTESIAN_POINT('Origin',(1.2,0.6,0.));
#8150=CARTESIAN_POINT('',(0.7,0.6,0.8));
#8151=CARTESIAN_POINT('',(0.7,0.6,-0.1));
#8152=CARTESIAN_POINT('Origin',(1.2,0.6,0.8));
#8153=CARTESIAN_POINT('Origin',(1.2,0.6,0.8));
#8154=CARTESIAN_POINT('',(0.925,0.6,0.8));
#8155=CARTESIAN_POINT('Origin',(1.2,0.6,0.8));
#8156=CARTESIAN_POINT('Origin',(-1.2,0.6,-0.1));
#8157=CARTESIAN_POINT('',(-1.475,0.6,2.));
#8158=CARTESIAN_POINT('',(-1.475,0.6,-0.1));
#8159=CARTESIAN_POINT('Origin',(-1.2,0.6,2.));
#8160=CARTESIAN_POINT('Origin',(1.2,0.6,-0.1));
#8161=CARTESIAN_POINT('',(0.925,0.6,2.));
#8162=CARTESIAN_POINT('',(0.925,0.6,-0.1));
#8163=CARTESIAN_POINT('Origin',(1.2,0.6,2.));
#8164=CARTESIAN_POINT('Origin',(3.5,1.8,0.));
#8165=CARTESIAN_POINT('',(3.5,1.8,0.));
#8166=CARTESIAN_POINT('',(-3.5,1.8,0.));
#8167=CARTESIAN_POINT('',(3.5,1.8,0.));
#8168=CARTESIAN_POINT('',(-3.5,1.8,2.));
#8169=CARTESIAN_POINT('',(-3.5,1.8,0.));
#8170=CARTESIAN_POINT('',(3.5,1.8,2.));
#8171=CARTESIAN_POINT('',(3.5,1.8,2.));
#8172=CARTESIAN_POINT('',(3.5,1.8,0.));
#8173=CARTESIAN_POINT('Origin',(3.5,0.,0.));
#8174=CARTESIAN_POINT('',(3.5,0.,0.));
#8175=CARTESIAN_POINT('',(3.5,0.,0.));
#8176=CARTESIAN_POINT('',(3.5,0.,2.));
#8177=CARTESIAN_POINT('',(3.5,0.,2.));
#8178=CARTESIAN_POINT('',(3.5,0.,0.));
#8179=CARTESIAN_POINT('Origin',(-3.5,0.,0.));
#8180=CARTESIAN_POINT('',(-3.5,0.,0.));
#8181=CARTESIAN_POINT('',(-3.5,0.,0.));
#8182=CARTESIAN_POINT('',(-3.5,0.,2.));
#8183=CARTESIAN_POINT('',(-3.5,0.,2.));
#8184=CARTESIAN_POINT('',(-3.5,0.,0.));
#8185=CARTESIAN_POINT('Origin',(-3.5,1.8,0.));
#8186=CARTESIAN_POINT('',(-3.5,1.8,0.));
#8187=CARTESIAN_POINT('',(-3.5,1.8,2.));
#8188=CARTESIAN_POINT('Origin',(0.,0.9,2.));
#8189=CARTESIAN_POINT('Origin',(0.,0.9,0.));
#8190=CARTESIAN_POINT('',(0.,0.,0.));
#8191=CARTESIAN_POINT('Origin',(0.375,0.5,0.));
#8192=CARTESIAN_POINT('',(-0.375,0.5,-4.59242549680257E-17));
#8193=CARTESIAN_POINT('Origin',(0.,0.5,0.));
#8194=CARTESIAN_POINT('Origin',(0.,0.475,0.));
#8195=CARTESIAN_POINT('',(-0.425,0.45,-5.20474889637625E-17));
#8196=CARTESIAN_POINT('Origin',(0.,0.45,0.));
#8197=CARTESIAN_POINT('',(-0.4,0.475,-4.89858719658941E-17));
#8198=CARTESIAN_POINT('Origin',(0.,0.24,0.));
#8199=CARTESIAN_POINT('',(-0.425,0.0299999999999998,-5.20474889637625E-17));
#8200=CARTESIAN_POINT('Origin',(0.,0.0299999999999998,0.));
#8201=CARTESIAN_POINT('',(-0.425,0.24,-5.20474889637625E-17));
#8202=CARTESIAN_POINT('Origin',(0.,0.0150000000000001,0.));
#8203=CARTESIAN_POINT('',(-0.395,4.85722573273506E-17,-4.83735485663204E-17));
#8204=CARTESIAN_POINT('Origin',(0.,0.,0.));
#8205=CARTESIAN_POINT('',(-0.41,0.0150000000000001,-5.02105187650415E-17));
#8206=CARTESIAN_POINT('Origin',(0.27,0.,0.));
#8207=CARTESIAN_POINT('',(-0.27,0.,-3.30654635769785E-17));
#8208=CARTESIAN_POINT('Origin',(0.,0.,0.));
#8209=CARTESIAN_POINT('Origin',(0.,-0.02,0.));
#8210=CARTESIAN_POINT('',(-0.24505,-0.0498999999999999,3.00099698131059E-17));
#8211=CARTESIAN_POINT('Origin',(0.,-0.0498999999999999,0.));
#8212=CARTESIAN_POINT('',(-0.26,-0.02,-3.18408167778312E-17));
#8213=CARTESIAN_POINT('Origin',(0.,-0.995,0.));
#8214=CARTESIAN_POINT('',(-0.24505,-1.95495,3.00099698131059E-17));
#8215=CARTESIAN_POINT('Origin',(0.,-1.95495,0.));
#8216=CARTESIAN_POINT('',(-0.24505,-0.995,-3.00099698131059E-17));
#8217=CARTESIAN_POINT('Origin',(0.,-1.975,0.));
#8218=CARTESIAN_POINT('',(-0.2,-2.,-2.44929359829471E-17));
#8219=CARTESIAN_POINT('Origin',(0.,-2.,0.));
#8220=CARTESIAN_POINT('',(-0.225,-1.975,-2.75545529808154E-17));
#8221=CARTESIAN_POINT('Origin',(0.,-2.,0.));
#8222=CARTESIAN_POINT('Origin',(0.115470053837925,-0.5,-0.2));
#8223=CARTESIAN_POINT('',(0.23094010767585,-0.5,0.));
#8224=CARTESIAN_POINT('',(0.115470053837925,-0.5,-0.2));
#8225=CARTESIAN_POINT('',(0.23094010767585,-0.5,0.));
#8226=CARTESIAN_POINT('',(0.115470053837925,-0.8,-0.2));
#8227=CARTESIAN_POINT('',(0.115470053837925,-0.5,-0.2));
#8228=CARTESIAN_POINT('',(0.23094010767585,-0.8,0.));
#8229=CARTESIAN_POINT('',(0.23094010767585,-0.8,0.));
#8230=CARTESIAN_POINT('',(0.23094010767585,-0.5,0.));
#8231=CARTESIAN_POINT('Origin',(-0.115470053837925,-0.5,-0.2));
#8232=CARTESIAN_POINT('',(-0.115470053837925,-0.5,-0.2));
#8233=CARTESIAN_POINT('',(0.115470053837925,-0.5,-0.2));
#8234=CARTESIAN_POINT('',(-0.115470053837925,-0.8,-0.2));
#8235=CARTESIAN_POINT('',(-0.115470053837925,-0.5,-0.2));
#8236=CARTESIAN_POINT('',(0.115470053837925,-0.8,-0.2));
#8237=CARTESIAN_POINT('Origin',(-0.23094010767585,-0.5,-2.77555756156289E-17));
#8238=CARTESIAN_POINT('',(-0.23094010767585,-0.5,-2.82820063659975E-17));
#8239=CARTESIAN_POINT('',(-0.115470053837925,-0.5,-0.2));
#8240=CARTESIAN_POINT('',(-0.23094010767585,-0.8,-2.77555756156289E-17));
#8241=CARTESIAN_POINT('',(-0.23094010767585,-0.5,-2.82820063659975E-17));
#8242=CARTESIAN_POINT('',(-0.115470053837925,-0.8,-0.2));
#8243=CARTESIAN_POINT('Origin',(-0.115470053837925,-0.5,0.2));
#8244=CARTESIAN_POINT('',(-0.115470053837925,-0.5,0.2));
#8245=CARTESIAN_POINT('',(-0.23094010767585,-0.5,-2.82820063659975E-17));
#8246=CARTESIAN_POINT('',(-0.115470053837925,-0.8,0.2));
#8247=CARTESIAN_POINT('',(-0.115470053837925,-0.5,0.2));
#8248=CARTESIAN_POINT('',(-0.23094010767585,-0.8,-2.82820063659975E-17));
#8249=CARTESIAN_POINT('Origin',(0.115470053837925,-0.5,0.2));
#8250=CARTESIAN_POINT('',(0.115470053837925,-0.5,0.2));
#8251=CARTESIAN_POINT('',(-0.115470053837925,-0.5,0.2));
#8252=CARTESIAN_POINT('',(0.115470053837925,-0.8,0.2));
#8253=CARTESIAN_POINT('',(0.115470053837925,-0.5,0.2));
#8254=CARTESIAN_POINT('',(-0.115470053837925,-0.8,0.2));
#8255=CARTESIAN_POINT('Origin',(0.23094010767585,-0.5,0.));
#8256=CARTESIAN_POINT('',(0.115470053837925,-0.5,0.2));
#8257=CARTESIAN_POINT('',(0.115470053837925,-0.8,0.2));
#8258=CARTESIAN_POINT('Origin',(0.,-0.5,0.));
#8259=CARTESIAN_POINT('Origin',(0.,-0.8,0.));
#8260=CARTESIAN_POINT('',(0.,0.,0.));
#8261=CARTESIAN_POINT('',(0.,0.,0.));
#8262=CARTESIAN_POINT('Origin',(0.,0.6,0.));
#8263=CARTESIAN_POINT('',(-0.43,0.6,5.26598123633362E-17));
#8264=CARTESIAN_POINT('Origin',(0.,0.6,0.));
#8265=CARTESIAN_POINT('',(-0.43,0.7,-5.26598123633362E-17));
#8266=CARTESIAN_POINT('',(-0.43,0.6,5.26598123633362E-17));
#8267=CARTESIAN_POINT('Origin',(0.,0.7,0.));
#8268=CARTESIAN_POINT('Origin',(0.,0.6,0.));
#8269=CARTESIAN_POINT('',(-0.2,0.6,2.44929359829471E-17));
#8270=CARTESIAN_POINT('Origin',(0.,0.6,0.));
#8271=CARTESIAN_POINT('Origin',(0.,0.5,-1.11022302462516E-16));
#8272=CARTESIAN_POINT('',(0.346410161513776,0.5,0.6));
#8273=CARTESIAN_POINT('',(0.692820323027551,0.5,0.));
#8274=CARTESIAN_POINT('',(0.346410161513776,0.5,0.6));
#8275=CARTESIAN_POINT('',(0.346410161513776,0.5,-0.6));
#8276=CARTESIAN_POINT('',(0.692820323027551,0.5,0.));
#8277=CARTESIAN_POINT('',(-0.346410161513775,0.5,-0.6));
#8278=CARTESIAN_POINT('',(0.346410161513776,0.5,-0.6));
#8279=CARTESIAN_POINT('',(-0.692820323027551,0.5,-8.48460190979926E-17));
#8280=CARTESIAN_POINT('',(-0.346410161513775,0.5,-0.6));
#8281=CARTESIAN_POINT('',(-0.346410161513776,0.5,0.6));
#8282=CARTESIAN_POINT('',(-0.692820323027551,0.5,-8.48460190979926E-17));
#8283=CARTESIAN_POINT('',(-0.346410161513776,0.5,0.6));
#8284=CARTESIAN_POINT('',(-0.525,0.5,-6.4293956955236E-17));
#8285=CARTESIAN_POINT('Origin',(0.,0.5,0.));
#8286=CARTESIAN_POINT('Origin',(0.,0.,-1.11022302462516E-16));
#8287=CARTESIAN_POINT('',(0.346410161513776,0.,0.6));
#8288=CARTESIAN_POINT('',(0.692820323027551,0.,0.));
#8289=CARTESIAN_POINT('',(0.346410161513776,0.,0.6));
#8290=CARTESIAN_POINT('',(-0.346410161513776,0.,0.6));
#8291=CARTESIAN_POINT('',(-0.346410161513776,0.,0.6));
#8292=CARTESIAN_POINT('',(-0.692820323027551,0.,-8.48460190979926E-17));
#8293=CARTESIAN_POINT('',(-0.692820323027551,0.,-8.48460190979926E-17));
#8294=CARTESIAN_POINT('',(-0.346410161513775,0.,-0.6));
#8295=CARTESIAN_POINT('',(-0.346410161513775,0.,-0.6));
#8296=CARTESIAN_POINT('',(0.346410161513776,0.,-0.6));
#8297=CARTESIAN_POINT('',(0.346410161513776,0.,-0.6));
#8298=CARTESIAN_POINT('',(0.692820323027551,0.,0.));
#8299=CARTESIAN_POINT('',(-0.515,0.,-6.30693101560887E-17));
#8300=CARTESIAN_POINT('Origin',(0.,0.,0.));
#8301=CARTESIAN_POINT('Origin',(-0.346410161513776,0.,0.6));
#8302=CARTESIAN_POINT('',(0.346410161513776,0.,0.6));
#8303=CARTESIAN_POINT('',(-0.346410161513776,0.,0.6));
#8304=CARTESIAN_POINT('Origin',(-0.692820323027551,0.,-8.48460190979926E-17));
#8305=CARTESIAN_POINT('',(-0.692820323027551,0.,-8.48460190979926E-17));
#8306=CARTESIAN_POINT('Origin',(-0.346410161513775,0.,-0.6));
#8307=CARTESIAN_POINT('',(-0.346410161513775,0.,-0.6));
#8308=CARTESIAN_POINT('Origin',(0.346410161513776,0.,-0.6));
#8309=CARTESIAN_POINT('',(0.346410161513776,0.,-0.6));
#8310=CARTESIAN_POINT('Origin',(0.692820323027551,0.,0.));
#8311=CARTESIAN_POINT('',(0.692820323027551,0.,0.));
#8312=CARTESIAN_POINT('Origin',(0.346410161513776,0.,0.6));
#8313=CARTESIAN_POINT('Origin',(0.46,0.7,0.));
#8314=CARTESIAN_POINT('',(-0.46,0.7,-5.63337527607782E-17));
#8315=CARTESIAN_POINT('Origin',(0.,0.7,0.));
#8316=CARTESIAN_POINT('Origin',(0.,1.2,0.));
#8317=CARTESIAN_POINT('',(-0.46,1.7,-5.63337527607782E-17));
#8318=CARTESIAN_POINT('',(-0.46,1.2,-5.63337527607782E-17));
#8319=CARTESIAN_POINT('Origin',(0.,1.7,0.));
#8320=CARTESIAN_POINT('Origin',(0.525,1.7,0.));
#8321=CARTESIAN_POINT('',(-0.525,1.7,-6.4293956955236E-17));
#8322=CARTESIAN_POINT('Origin',(0.,1.7,0.));
#8323=CARTESIAN_POINT('Origin',(0.,1.1,0.));
#8324=CARTESIAN_POINT('',(-0.525,1.1,-6.4293956955236E-17));
#8325=CARTESIAN_POINT('Origin',(0.,-0.325,0.));
#8326=CARTESIAN_POINT('',(-0.515,-0.65,-6.30693101560887E-17));
#8327=CARTESIAN_POINT('Origin',(0.,-0.65,0.));
#8328=CARTESIAN_POINT('',(-0.515,-0.325,-6.30693101560887E-17));
#8329=CARTESIAN_POINT('Origin',(0.2,-0.65,0.));
#8330=CARTESIAN_POINT('',(-0.2,-0.65,-2.44929359829471E-17));
#8331=CARTESIAN_POINT('Origin',(0.,-0.65,0.));
#8332=CARTESIAN_POINT('Origin',(0.,0.0249999999999999,0.));
#8333=CARTESIAN_POINT('',(-0.2,0.0249999999999999,-2.44929359829471E-17));
#8334=CARTESIAN_POINT('',(0.,0.,0.));
#8335=CARTESIAN_POINT('Origin',(0.475,1.95,0.));
#8336=CARTESIAN_POINT('',(-0.475,1.95,-5.81707229594993E-17));
#8337=CARTESIAN_POINT('Origin',(0.,1.95,0.));
#8338=CARTESIAN_POINT('',(-0.31,1.95,-3.7964050773568E-17));
#8339=CARTESIAN_POINT('Origin',(0.,1.95,0.));
#8340=CARTESIAN_POINT('Origin',(0.,1.825,0.));
#8341=CARTESIAN_POINT('',(-0.475,1.7,-5.81707229594993E-17));
#8342=CARTESIAN_POINT('Origin',(0.,1.7,0.));
#8343=CARTESIAN_POINT('',(-0.475,1.825,-5.81707229594993E-17));
#8344=CARTESIAN_POINT('Origin',(0.355,1.7,0.));
#8345=CARTESIAN_POINT('',(-0.355,1.7,-4.3474961369731E-17));
#8346=CARTESIAN_POINT('Origin',(0.,1.7,0.));
#8347=CARTESIAN_POINT('Origin',(0.,1.55,0.));
#8348=CARTESIAN_POINT('',(-0.355,1.4,-4.3474961369731E-17));
#8349=CARTESIAN_POINT('Origin',(0.,1.4,0.));
#8350=CARTESIAN_POINT('',(-0.355,1.55,-4.3474961369731E-17));
#8351=CARTESIAN_POINT('Origin',(0.31,1.4,0.));
#8352=CARTESIAN_POINT('',(-0.31,1.4,-3.7964050773568E-17));
#8353=CARTESIAN_POINT('Origin',(0.,1.4,0.));
#8354=CARTESIAN_POINT('Origin',(0.,1.675,0.));
#8355=CARTESIAN_POINT('',(-0.31,1.675,-3.7964050773568E-17));
#8356=CARTESIAN_POINT('',(0.,0.,0.));
#8357=CARTESIAN_POINT('',(0.,0.,0.));
#8358=CARTESIAN_POINT('',(0.,0.,0.));
#8359=CARTESIAN_POINT('Origin',(0.,0.,0.));
#8360=CARTESIAN_POINT('',(-3.71680303541222E-17,-1.08993565124114E-17,0.3035));
#8361=CARTESIAN_POINT('Origin',(-4.80673868665336E-17,0.,0.3925));
#8362=CARTESIAN_POINT('Origin',(0.,1.08993565124114E-17,0.));
#8363=CARTESIAN_POINT('',(0.,0.,0.));
#8364=CARTESIAN_POINT('Origin',(0.,0.125,4.5));
#8365=CARTESIAN_POINT('',(-0.51,0.125,4.5));
#8366=CARTESIAN_POINT('Origin',(0.,0.125,4.5));
#8367=CARTESIAN_POINT('',(-0.51,0.275,4.5));
#8368=CARTESIAN_POINT('',(-0.51,0.125,4.5));
#8369=CARTESIAN_POINT('Origin',(0.,0.275,4.5));
#8370=CARTESIAN_POINT('Origin',(0.,0.275,4.5));
#8371=CARTESIAN_POINT('',(-0.405,0.275,4.5));
#8372=CARTESIAN_POINT('Origin',(0.,0.275,4.5));
#8373=CARTESIAN_POINT('Origin',(0.,0.125,4.5));
#8374=CARTESIAN_POINT('',(-0.405,0.125,4.5));
#8375=CARTESIAN_POINT('Origin',(0.,0.125,4.5));
#8376=CARTESIAN_POINT('Origin',(0.,0.,4.5));
#8377=CARTESIAN_POINT('',(-0.405,0.,4.5));
#8378=CARTESIAN_POINT('',(-0.405,0.,4.5));
#8379=CARTESIAN_POINT('Origin',(0.,0.,4.5));
#8380=CARTESIAN_POINT('Origin',(0.,0.,4.5));
#8381=CARTESIAN_POINT('',(-0.405,1.2,4.5));
#8382=CARTESIAN_POINT('Origin',(0.,1.2,4.5));
#8383=CARTESIAN_POINT('',(-0.405,0.,4.5));
#8384=CARTESIAN_POINT('Origin',(0.,0.,4.5));
#8385=CARTESIAN_POINT('',(-0.6,1.2,4.5));
#8386=CARTESIAN_POINT('Origin',(0.,1.2,4.5));
#8387=CARTESIAN_POINT('',(-0.6,0.,4.5));
#8388=CARTESIAN_POINT('',(-0.6,0.,4.5));
#8389=CARTESIAN_POINT('Origin',(0.,0.,4.5));
#8390=CARTESIAN_POINT('Origin',(0.,1.2,4.5));
#8391=CARTESIAN_POINT('Origin',(0.,0.,4.5));
#8392=CARTESIAN_POINT('',(0.,0.,0.));
#8393=CARTESIAN_POINT('Origin',(0.,0.2,4.5));
#8394=CARTESIAN_POINT('',(-4.89858719658941E-17,0.2,4.9));
#8395=CARTESIAN_POINT('Origin',(-5.51091059616309E-17,0.2,4.95));
#8396=CARTESIAN_POINT('Origin',(0.,0.2,4.5));
#8397=CARTESIAN_POINT('',(0.,0.,0.));
#8398=CARTESIAN_POINT('Origin',(-2.,-1.,2.5));
#8399=CARTESIAN_POINT('',(-2.25,13.6,2.5));
#8400=CARTESIAN_POINT('Origin',(-2.,13.6,2.5));
#8401=CARTESIAN_POINT('',(-2.25,-1.,2.5));
#8402=CARTESIAN_POINT('',(-2.25,-1.,2.5));
#8403=CARTESIAN_POINT('Origin',(-2.,-1.,2.5));
#8404=CARTESIAN_POINT('Origin',(-2.,13.6,2.5));
#8405=CARTESIAN_POINT('Origin',(-2.,-1.,2.5));
#8406=CARTESIAN_POINT('',(0.,0.,0.));
#8407=CARTESIAN_POINT('Origin',(0.,0.09,0.));
#8408=CARTESIAN_POINT('',(-0.285,0.1,3.49024337756996E-17));
#8409=CARTESIAN_POINT('Origin',(0.,0.1,0.));
#8410=CARTESIAN_POINT('',(-0.265,0.08,-3.24531401774049E-17));
#8411=CARTESIAN_POINT('',(-0.275,0.09,3.36777869765522E-17));
#8412=CARTESIAN_POINT('Origin',(0.,0.08,0.));
#8413=CARTESIAN_POINT('Origin',(0.,0.,0.));
#8414=CARTESIAN_POINT('',(-0.265,0.,3.24531401774049E-17));
#8415=CARTESIAN_POINT('',(-0.265,0.,3.24531401774049E-17));
#8416=CARTESIAN_POINT('Origin',(0.,0.,0.));
#8417=CARTESIAN_POINT('Origin',(0.,0.1,0.));
#8418=CARTESIAN_POINT('',(-0.5,0.1,6.12323399573677E-17));
#8419=CARTESIAN_POINT('Origin',(0.,0.1,0.));
#8420=CARTESIAN_POINT('Origin',(0.,0.,0.));
#8421=CARTESIAN_POINT('',(-0.5,0.,6.12323399573677E-17));
#8422=CARTESIAN_POINT('',(-0.5,0.,6.12323399573677E-17));
#8423=CARTESIAN_POINT('Origin',(0.,0.,0.));
#8424=CARTESIAN_POINT('Origin',(0.,0.,0.));
#8425=CARTESIAN_POINT('',(0.,0.,0.));
#8426=CARTESIAN_POINT('Origin',(0.,0.0525042956467857,0.));
#8427=CARTESIAN_POINT('',(-0.230940107675851,0.0472735643746089,0.4));
#8428=CARTESIAN_POINT('',(0.23094010767585,0.0472735643746089,0.4));
#8429=CARTESIAN_POINT('Ctrl Pts',(-0.230940107675851,0.0472735643746089,
0.4));
#8430=CARTESIAN_POINT('Ctrl Pts',(1.11022302462516E-16,-0.0193931022920578,
0.4));
#8431=CARTESIAN_POINT('Ctrl Pts',(0.23094010767585,0.0472735643746089,0.4));
#8432=CARTESIAN_POINT('',(-0.461880215351701,0.0472735643746089,-5.6564012731995E-17));
#8433=CARTESIAN_POINT('Ctrl Pts',(-0.461880215351701,0.0472735643746089,
-5.6564012731995E-17));
#8434=CARTESIAN_POINT('Ctrl Pts',(-0.346410161513776,-0.0193931022920579,
0.2));
#8435=CARTESIAN_POINT('Ctrl Pts',(-0.230940107675851,0.0472735643746089,
0.4));
#8436=CARTESIAN_POINT('',(-0.38,-2.08166817117217E-17,-4.65365783675994E-17));
#8437=CARTESIAN_POINT('',(-0.47094010767585,0.0525042956467857,-5.7673529545534E-17));
#8438=CARTESIAN_POINT('Origin',(0.,0.,0.));
#8439=CARTESIAN_POINT('',(-0.23094010767585,0.0472735643746089,-0.4));
#8440=CARTESIAN_POINT('Ctrl Pts',(-0.23094010767585,0.0472735643746089,
-0.4));
#8441=CARTESIAN_POINT('Ctrl Pts',(-0.346410161513775,-0.0193931022920578,
-0.2));
#8442=CARTESIAN_POINT('Ctrl Pts',(-0.461880215351701,0.0472735643746089,
-5.6564012731995E-17));
#8443=CARTESIAN_POINT('',(0.23094010767585,0.0472735643746089,-0.4));
#8444=CARTESIAN_POINT('Ctrl Pts',(0.23094010767585,0.0472735643746089,-0.4));
#8445=CARTESIAN_POINT('Ctrl Pts',(0.,-0.0193931022920578,-0.4));
#8446=CARTESIAN_POINT('Ctrl Pts',(-0.23094010767585,0.0472735643746089,
-0.4));
#8447=CARTESIAN_POINT('',(0.461880215351701,0.0472735643746089,0.));
#8448=CARTESIAN_POINT('Ctrl Pts',(0.461880215351701,0.0472735643746089,
0.));
#8449=CARTESIAN_POINT('Ctrl Pts',(0.346410161513776,-0.019393102292058,
-0.2));
#8450=CARTESIAN_POINT('Ctrl Pts',(0.23094010767585,0.0472735643746089,-0.4));
#8451=CARTESIAN_POINT('Ctrl Pts',(0.23094010767585,0.0472735643746089,0.4));
#8452=CARTESIAN_POINT('Ctrl Pts',(0.346410161513776,-0.0193931022920577,
0.2));
#8453=CARTESIAN_POINT('Ctrl Pts',(0.461880215351701,0.0472735643746089,
0.));
#8454=CARTESIAN_POINT('Origin',(0.,0.417495704353214,0.));
#8455=CARTESIAN_POINT('',(-0.38,0.47,-4.65365783675994E-17));
#8456=CARTESIAN_POINT('Origin',(0.,0.47,0.));
#8457=CARTESIAN_POINT('',(-0.461880215351701,0.422726435625391,-5.6564012731995E-17));
#8458=CARTESIAN_POINT('',(-0.47094010767585,0.417495704353214,-5.7673529545534E-17));
#8459=CARTESIAN_POINT('',(-0.230940107675851,0.422726435625391,0.4));
#8460=CARTESIAN_POINT('Ctrl Pts',(-0.230940107675851,0.422726435625391,
0.4));
#8461=CARTESIAN_POINT('Ctrl Pts',(-0.346410161513776,0.489393102292058,
0.2));
#8462=CARTESIAN_POINT('Ctrl Pts',(-0.461880215351701,0.422726435625391,
-5.6564012731995E-17));
#8463=CARTESIAN_POINT('',(0.23094010767585,0.422726435625391,0.4));
#8464=CARTESIAN_POINT('Ctrl Pts',(0.23094010767585,0.422726435625391,0.4));
#8465=CARTESIAN_POINT('Ctrl Pts',(8.32667268468867E-17,0.489393102292058,
0.4));
#8466=CARTESIAN_POINT('Ctrl Pts',(-0.230940107675851,0.422726435625391,
0.4));
#8467=CARTESIAN_POINT('',(0.461880215351701,0.422726435625391,0.));
#8468=CARTESIAN_POINT('Ctrl Pts',(0.461880215351701,0.422726435625391,0.));
#8469=CARTESIAN_POINT('Ctrl Pts',(0.346410161513776,0.489393102292058,0.2));
#8470=CARTESIAN_POINT('Ctrl Pts',(0.23094010767585,0.422726435625391,0.4));
#8471=CARTESIAN_POINT('',(0.23094010767585,0.422726435625391,-0.4));
#8472=CARTESIAN_POINT('Ctrl Pts',(0.23094010767585,0.422726435625391,-0.4));
#8473=CARTESIAN_POINT('Ctrl Pts',(0.346410161513775,0.489393102292058,-0.2));
#8474=CARTESIAN_POINT('Ctrl Pts',(0.461880215351701,0.422726435625391,0.));
#8475=CARTESIAN_POINT('',(-0.23094010767585,0.422726435625391,-0.4));
#8476=CARTESIAN_POINT('Ctrl Pts',(-0.23094010767585,0.422726435625391,-0.4));
#8477=CARTESIAN_POINT('Ctrl Pts',(-5.55111512312578E-17,0.489393102292058,
-0.4));
#8478=CARTESIAN_POINT('Ctrl Pts',(0.23094010767585,0.422726435625391,-0.4));
#8479=CARTESIAN_POINT('Ctrl Pts',(-0.461880215351701,0.422726435625391,
-5.6564012731995E-17));
#8480=CARTESIAN_POINT('Ctrl Pts',(-0.346410161513776,0.489393102292058,
-0.2));
#8481=CARTESIAN_POINT('Ctrl Pts',(-0.23094010767585,0.422726435625391,-0.4));
#8482=CARTESIAN_POINT('Origin',(0.23094010767585,0.,-0.4));
#8483=CARTESIAN_POINT('',(-0.23094010767585,0.,-0.4));
#8484=CARTESIAN_POINT('',(0.23094010767585,0.,-0.4));
#8485=CARTESIAN_POINT('Origin',(-0.23094010767585,0.,-0.4));
#8486=CARTESIAN_POINT('',(-0.461880215351701,0.,-5.6564012731995E-17));
#8487=CARTESIAN_POINT('Origin',(-0.461880215351701,0.,-5.6564012731995E-17));
#8488=CARTESIAN_POINT('',(-0.230940107675851,0.,0.4));
#8489=CARTESIAN_POINT('Origin',(0.,0.,0.));
#8490=CARTESIAN_POINT('',(-0.2117,0.47,2.59257727379495E-17));
#8491=CARTESIAN_POINT('Origin',(0.,0.47,0.));
#8492=CARTESIAN_POINT('',(-0.2117,0.,2.59257727379495E-17));
#8493=CARTESIAN_POINT('',(-0.2117,0.,2.59257727379495E-17));
#8494=CARTESIAN_POINT('Origin',(0.,0.,0.));
#8495=CARTESIAN_POINT('Origin',(-0.230940107675851,0.,0.4));
#8496=CARTESIAN_POINT('',(0.23094010767585,0.,0.4));
#8497=CARTESIAN_POINT('Origin',(0.461880215351701,0.,0.));
#8498=CARTESIAN_POINT('',(0.461880215351701,0.,0.));
#8499=CARTESIAN_POINT('Origin',(0.23094010767585,0.,0.4));
#8500=CARTESIAN_POINT('Origin',(0.,0.47,0.));
#8501=CARTESIAN_POINT('Origin',(0.,0.,0.));
#8502=CARTESIAN_POINT('',(0.,0.,0.));
#8503=CARTESIAN_POINT('',(0.,0.,0.));
#8504=CARTESIAN_POINT('',(0.,0.,0.));
#8505=CARTESIAN_POINT('',(0.,0.,0.));
#8506=CARTESIAN_POINT('',(0.,0.,0.));
#8507=CARTESIAN_POINT('',(0.,0.,0.));
#8508=CARTESIAN_POINT('',(0.,0.,0.));
#8509=CARTESIAN_POINT('',(0.,0.,0.));
#8510=CARTESIAN_POINT('',(0.,0.,0.));
#8511=CARTESIAN_POINT('',(0.,0.,0.));
#8512=CARTESIAN_POINT('',(-1.2,0.6,0.8));
#8513=CARTESIAN_POINT('',(1.2,0.6,0.8));
#8514=CARTESIAN_POINT('',(1.,0.8,8.5));
#8515=CARTESIAN_POINT('',(0.,0.8,9.3));
#8516=CARTESIAN_POINT('',(0.,12.6,0.));
#8517=CARTESIAN_POINT('',(-1.2,12.,0.8));
#8518=CARTESIAN_POINT('',(1.2,12.,0.8));
#8519=CARTESIAN_POINT('',(1.,11.8,8.5));
#8520=CARTESIAN_POINT('',(0.,11.8,9.3));
#8521=CARTESIAN_POINT('',(0.,0.,0.));
#8522=CARTESIAN_POINT('',(0.,0.,0.));
#8523=CARTESIAN_POINT('',(0.,0.,0.));
#8524=CARTESIAN_POINT('',(-2.,0.,2.5));
#8525=CARTESIAN_POINT('',(-2.,-0.57,2.5));
#8526=CARTESIAN_POINT('',(-2.,12.6,2.5));
#8527=CARTESIAN_POINT('',(-2.,12.7,2.5));
#8528=CARTESIAN_POINT('',(0.,0.,4.));
#8529=CARTESIAN_POINT('',(-2.,0.,6.5));
#8530=CARTESIAN_POINT('',(-2.,-0.57,6.5));
#8531=CARTESIAN_POINT('',(-2.,12.6,6.5));
#8532=CARTESIAN_POINT('',(-2.,12.7,6.5));
#8533=CARTESIAN_POINT('',(4.,0.,0.));
#8534=CARTESIAN_POINT('',(2.,0.,2.5));
#8535=CARTESIAN_POINT('',(2.,-0.57,2.5));
#8536=CARTESIAN_POINT('',(2.,12.6,2.5));
#8537=CARTESIAN_POINT('',(2.,12.7,2.5));
#8538=CARTESIAN_POINT('',(4.,0.,4.));
#8539=CARTESIAN_POINT('',(2.,0.,6.5));
#8540=CARTESIAN_POINT('',(2.,-0.57,6.5));
#8541=CARTESIAN_POINT('',(2.,12.6,6.5));
#8542=CARTESIAN_POINT('',(2.,12.7,6.5));
#8543=CARTESIAN_POINT('',(0.,0.,0.));
#8544=CARTESIAN_POINT('',(0.,0.,0.));
#8545=CARTESIAN_POINT('Origin',(0.,3.2,4.5));
#8546=CARTESIAN_POINT('',(-0.4,3.2,4.5));
#8547=CARTESIAN_POINT('Origin',(0.,3.2,4.5));
#8548=CARTESIAN_POINT('',(-0.4,3.6,4.5));
#8549=CARTESIAN_POINT('',(-0.4,3.2,4.5));
#8550=CARTESIAN_POINT('Origin',(0.,3.6,4.5));
#8551=CARTESIAN_POINT('Origin',(0.,3.2,4.5));
#8552=CARTESIAN_POINT('',(-0.225,3.2,4.5));
#8553=CARTESIAN_POINT('Origin',(0.,3.2,4.5));
#8554=CARTESIAN_POINT('Origin',(0.,2.8,4.5));
#8555=CARTESIAN_POINT('',(-0.9,2.8,4.5));
#8556=CARTESIAN_POINT('Origin',(0.,2.8,4.5));
#8557=CARTESIAN_POINT('',(-0.9,3.1,4.5));
#8558=CARTESIAN_POINT('',(-0.9,2.8,4.5));
#8559=CARTESIAN_POINT('Origin',(0.,3.1,4.5));
#8560=CARTESIAN_POINT('Origin',(0.,3.1,4.5));
#8561=CARTESIAN_POINT('',(-0.99,3.1,4.5));
#8562=CARTESIAN_POINT('Origin',(0.,3.1,4.5));
#8563=CARTESIAN_POINT('Origin',(0.,2.8,4.5));
#8564=CARTESIAN_POINT('',(-0.99,2.8,4.5));
#8565=CARTESIAN_POINT('Origin',(0.,2.8,4.5));
#8566=CARTESIAN_POINT('Origin',(0.,2.4,4.5));
#8567=CARTESIAN_POINT('',(-0.99,2.4,4.5));
#8568=CARTESIAN_POINT('',(-0.99,2.4,4.5));
#8569=CARTESIAN_POINT('Origin',(0.,2.4,4.5));
#8570=CARTESIAN_POINT('Origin',(0.,2.4,4.5));
#8571=CARTESIAN_POINT('',(-0.225,2.4,4.5));
#8572=CARTESIAN_POINT('',(-0.225,2.4,4.5));
#8573=CARTESIAN_POINT('Origin',(0.,2.4,4.5));
#8574=CARTESIAN_POINT('Origin',(0.,2.4,4.5));
#8575=CARTESIAN_POINT('',(-0.99,3.6,4.5));
#8576=CARTESIAN_POINT('Origin',(0.,3.6,4.5));
#8577=CARTESIAN_POINT('',(-0.99,2.4,4.5));
#8578=CARTESIAN_POINT('Origin',(0.,3.6,4.5));
#8579=CARTESIAN_POINT('Origin',(0.,2.4,4.5));
#8580=CARTESIAN_POINT('',(0.,0.,0.));
#8581=CARTESIAN_POINT('Origin',(0.,2.95,4.5));
#8582=CARTESIAN_POINT('',(-1.10218211923262E-16,2.95,5.4));
#8583=CARTESIAN_POINT('Origin',(-1.16341445918999E-16,2.95,5.45));
#8584=CARTESIAN_POINT('Origin',(0.,2.95,4.5));
#8585=CARTESIAN_POINT('',(0.,0.,0.));
#8586=CARTESIAN_POINT('Origin',(0.,1.2,4.5));
#8587=CARTESIAN_POINT('',(-0.165,1.2,4.5));
#8588=CARTESIAN_POINT('Origin',(0.,1.2,4.5));
#8589=CARTESIAN_POINT('',(-0.165,2.4,4.5));
#8590=CARTESIAN_POINT('',(-0.165,1.2,4.5));
#8591=CARTESIAN_POINT('Origin',(0.,2.4,4.5));
#8592=CARTESIAN_POINT('Origin',(0.,1.2,4.5));
#8593=CARTESIAN_POINT('Origin',(0.,-5.6,4.5));
#8594=CARTESIAN_POINT('',(-0.4,2.4,4.5));
#8595=CARTESIAN_POINT('Origin',(0.,2.4,4.5));
#8596=CARTESIAN_POINT('',(-0.4,-5.6,4.5));
#8597=CARTESIAN_POINT('',(-0.4,-5.6,4.5));
#8598=CARTESIAN_POINT('Origin',(0.,-5.6,4.5));
#8599=CARTESIAN_POINT('Origin',(0.,2.4,4.5));
#8600=CARTESIAN_POINT('Origin',(0.,-5.6,4.5));
#8601=CARTESIAN_POINT('',(0.,0.,0.));
#8602=CARTESIAN_POINT('Origin',(0.3,0.4,0.));
#8603=CARTESIAN_POINT('',(-0.3,0.4,-3.67394039744206E-17));
#8604=CARTESIAN_POINT('Origin',(0.,0.4,0.));
#8605=CARTESIAN_POINT('Origin',(0.,0.375,0.));
#8606=CARTESIAN_POINT('',(-0.35,0.35,-4.28626379701573E-17));
#8607=CARTESIAN_POINT('Origin',(0.,0.35,0.));
#8608=CARTESIAN_POINT('',(-0.325,0.375,-3.9801020972289E-17));
#8609=CARTESIAN_POINT('Origin',(0.,0.19,0.));
#8610=CARTESIAN_POINT('',(-0.35,0.03,-4.28626379701574E-17));
#8611=CARTESIAN_POINT('Origin',(0.,0.03,0.));
#8612=CARTESIAN_POINT('',(-0.35,0.19,-4.28626379701574E-17));
#8613=CARTESIAN_POINT('Origin',(0.,0.0149999999999999,0.));
#8614=CARTESIAN_POINT('',(-0.32,-3.29597460435593E-17,-3.91886975727153E-17));
#8615=CARTESIAN_POINT('Origin',(0.,0.,0.));
#8616=CARTESIAN_POINT('',(-0.335,0.0149999999999999,-4.10256677714363E-17));
#8617=CARTESIAN_POINT('Origin',(0.22,0.,0.));
#8618=CARTESIAN_POINT('',(-0.22,-6.93889390390723E-18,-2.69422295812418E-17));
#8619=CARTESIAN_POINT('Origin',(0.,0.,0.));
#8620=CARTESIAN_POINT('Origin',(0.,-0.02,0.));
#8621=CARTESIAN_POINT('',(-0.1954,-0.0492,2.39295984553393E-17));
#8622=CARTESIAN_POINT('Origin',(0.,-0.0492,0.));
#8623=CARTESIAN_POINT('',(-0.21,-0.02,-2.57175827820944E-17));
#8624=CARTESIAN_POINT('Origin',(0.,-0.8,0.));
#8625=CARTESIAN_POINT('',(-0.1954,-1.5646,2.39295984553393E-17));
#8626=CARTESIAN_POINT('Origin',(0.,-1.5646,0.));
#8627=CARTESIAN_POINT('',(-0.1954,-0.8,-2.39295984553393E-17));
#8628=CARTESIAN_POINT('Origin',(0.,-1.58,0.));
#8629=CARTESIAN_POINT('',(-0.16,-1.6,-1.95943487863577E-17));
#8630=CARTESIAN_POINT('Origin',(0.,-1.6,0.));
#8631=CARTESIAN_POINT('',(-0.18,-1.58,-2.20436423846524E-17));
#8632=CARTESIAN_POINT('Origin',(0.,-1.6,0.));
#8633=CARTESIAN_POINT('Origin',(0.0866025403784439,-0.4,-0.15));
#8634=CARTESIAN_POINT('',(0.173205080756888,-0.4,0.));
#8635=CARTESIAN_POINT('',(0.0866025403784439,-0.4,-0.15));
#8636=CARTESIAN_POINT('',(0.173205080756888,-0.4,0.));
#8637=CARTESIAN_POINT('',(0.0866025403784439,-0.64,-0.15));
#8638=CARTESIAN_POINT('',(0.0866025403784439,-0.4,-0.15));
#8639=CARTESIAN_POINT('',(0.173205080756888,-0.64,0.));
#8640=CARTESIAN_POINT('',(0.173205080756888,-0.64,0.));
#8641=CARTESIAN_POINT('',(0.173205080756888,-0.4,0.));
#8642=CARTESIAN_POINT('Origin',(-0.0866025403784438,-0.4,-0.15));
#8643=CARTESIAN_POINT('',(-0.0866025403784438,-0.4,-0.15));
#8644=CARTESIAN_POINT('',(0.0866025403784439,-0.4,-0.15));
#8645=CARTESIAN_POINT('',(-0.0866025403784438,-0.64,-0.15));
#8646=CARTESIAN_POINT('',(-0.0866025403784438,-0.4,-0.15));
#8647=CARTESIAN_POINT('',(0.0866025403784439,-0.64,-0.15));
#8648=CARTESIAN_POINT('Origin',(-0.173205080756888,-0.4,-2.77555756156289E-17));
#8649=CARTESIAN_POINT('',(-0.173205080756888,-0.4,-2.12115047744981E-17));
#8650=CARTESIAN_POINT('',(-0.0866025403784438,-0.4,-0.15));
#8651=CARTESIAN_POINT('',(-0.173205080756888,-0.64,-2.77555756156289E-17));
#8652=CARTESIAN_POINT('',(-0.173205080756888,-0.4,-2.12115047744981E-17));
#8653=CARTESIAN_POINT('',(-0.0866025403784438,-0.64,-0.15));
#8654=CARTESIAN_POINT('Origin',(-0.0866025403784439,-0.4,0.15));
#8655=CARTESIAN_POINT('',(-0.0866025403784439,-0.4,0.15));
#8656=CARTESIAN_POINT('',(-0.173205080756888,-0.4,-2.12115047744981E-17));
#8657=CARTESIAN_POINT('',(-0.0866025403784439,-0.64,0.15));
#8658=CARTESIAN_POINT('',(-0.0866025403784439,-0.4,0.15));
#8659=CARTESIAN_POINT('',(-0.173205080756888,-0.64,-2.12115047744981E-17));
#8660=CARTESIAN_POINT('Origin',(0.0866025403784439,-0.4,0.15));
#8661=CARTESIAN_POINT('',(0.0866025403784439,-0.4,0.15));
#8662=CARTESIAN_POINT('',(-0.0866025403784439,-0.4,0.15));
#8663=CARTESIAN_POINT('',(0.0866025403784439,-0.64,0.15));
#8664=CARTESIAN_POINT('',(0.0866025403784439,-0.4,0.15));
#8665=CARTESIAN_POINT('',(-0.0866025403784439,-0.64,0.15));
#8666=CARTESIAN_POINT('Origin',(0.173205080756888,-0.4,0.));
#8667=CARTESIAN_POINT('',(0.0866025403784439,-0.4,0.15));
#8668=CARTESIAN_POINT('',(0.0866025403784439,-0.64,0.15));
#8669=CARTESIAN_POINT('Origin',(0.,-0.4,-2.77555756156289E-17));
#8670=CARTESIAN_POINT('Origin',(0.,-0.64,-2.77555756156289E-17));
#8671=CARTESIAN_POINT('',(0.,0.,0.));
#8672=CARTESIAN_POINT('Origin',(-1.1,-6.1,4.5));
#8673=CARTESIAN_POINT('',(-1.,-6.1,4.805));
#8674=CARTESIAN_POINT('Origin',(-1.,-6.1,4.5));
#8675=CARTESIAN_POINT('',(-0.5,-6.1,4.805));
#8676=CARTESIAN_POINT('',(-1.1,-6.1,4.805));
#8677=CARTESIAN_POINT('Origin',(-0.5,-6.1,4.5));
#8678=CARTESIAN_POINT('Origin',(-1.1,-6.1,4.5));
#8679=CARTESIAN_POINT('',(0.5,-6.1,4.805));
#8680=CARTESIAN_POINT('Origin',(0.5,-6.1,4.5));
#8681=CARTESIAN_POINT('',(1.,-6.1,4.805));
#8682=CARTESIAN_POINT('',(-1.1,-6.1,4.805));
#8683=CARTESIAN_POINT('Origin',(1.,-6.1,4.5));
#8684=CARTESIAN_POINT('Origin',(0.,-5.3,4.89));
#8685=CARTESIAN_POINT('',(0.0888819441731535,-5.43901438774458,4.89));
#8686=CARTESIAN_POINT('',(0.0888819441731535,-5.16098561225542,4.89));
#8687=CARTESIAN_POINT('',(0.0888819441731535,-5.6,4.89));
#8688=CARTESIAN_POINT('Origin',(0.,-5.3,4.89));
#8689=CARTESIAN_POINT('Origin',(0.,-5.3,4.89));
#8690=CARTESIAN_POINT('',(-0.0888819441731535,-5.43901438774458,4.89));
#8691=CARTESIAN_POINT('Ctrl Pts',(-0.0888819441731541,-5.43901438774458,
4.89));
#8692=CARTESIAN_POINT('Ctrl Pts',(-0.0808964434200148,-5.44412009546053,
4.89181991495419));
#8693=CARTESIAN_POINT('Ctrl Pts',(-0.0723643333023662,-5.44859639186021,
4.89350251788328));
#8694=CARTESIAN_POINT('Ctrl Pts',(-0.0431949313468613,-5.46075622416973,
4.89819171553211));
#8695=CARTESIAN_POINT('Ctrl Pts',(-0.0209808024963256,-5.465,4.9));
#8696=CARTESIAN_POINT('Ctrl Pts',(0.0209808024963256,-5.465,4.9));
#8697=CARTESIAN_POINT('Ctrl Pts',(0.0431949313468613,-5.46075622416973,
4.89819171553211));
#8698=CARTESIAN_POINT('Ctrl Pts',(0.0723643333023662,-5.44859639186021,
4.89350251788328));
#8699=CARTESIAN_POINT('Ctrl Pts',(0.0808964434200144,-5.44412009546053,
4.89181991495419));
#8700=CARTESIAN_POINT('Ctrl Pts',(0.0888819441731541,-5.43901438774458,
4.89));
#8701=CARTESIAN_POINT('',(-0.165,-5.3,4.89));
#8702=CARTESIAN_POINT('Origin',(0.,-5.3,4.89));
#8703=CARTESIAN_POINT('',(-0.165,-5.3,5.5));
#8704=CARTESIAN_POINT('',(-0.165,-5.3,4.89));
#8705=CARTESIAN_POINT('Origin',(0.,-5.3,5.5));
#8706=CARTESIAN_POINT('',(-0.0888819441731535,-5.16098561225542,4.89));
#8707=CARTESIAN_POINT('Origin',(0.,-5.3,4.89));
#8708=CARTESIAN_POINT('Ctrl Pts',(0.0888819441731536,-5.16098561225542,
4.89));
#8709=CARTESIAN_POINT('Ctrl Pts',(0.0808964434200141,-5.15587990453947,
4.89181991495419));
#8710=CARTESIAN_POINT('Ctrl Pts',(0.0723643333023662,-5.15140360813979,
4.89350251788328));
#8711=CARTESIAN_POINT('Ctrl Pts',(0.0431949313468613,-5.13924377583027,
4.89819171553211));
#8712=CARTESIAN_POINT('Ctrl Pts',(0.0209808024963256,-5.135,4.9));
#8713=CARTESIAN_POINT('Ctrl Pts',(-0.0209808024963256,-5.135,4.9));
#8714=CARTESIAN_POINT('Ctrl Pts',(-0.0431949313468613,-5.13924377583027,
4.89819171553211));
#8715=CARTESIAN_POINT('Ctrl Pts',(-0.0723643333023663,-5.15140360813979,
4.89350251788328));
#8716=CARTESIAN_POINT('Ctrl Pts',(-0.0808964434200144,-5.15587990453947,
4.89181991495419));
#8717=CARTESIAN_POINT('Ctrl Pts',(-0.0888819441731536,-5.16098561225542,
4.89));
#8718=CARTESIAN_POINT('Origin',(0.,-5.3,4.89));
#8719=CARTESIAN_POINT('',(-0.0888819441731535,-5.6,4.89));
#8720=CARTESIAN_POINT('Origin',(0.,-5.6,4.5));
#8721=CARTESIAN_POINT('',(-0.4,-5.6,4.5));
#8722=CARTESIAN_POINT('Origin',(0.,-5.6,4.5));
#8723=CARTESIAN_POINT('',(-0.4,-5.,4.5));
#8724=CARTESIAN_POINT('',(-0.4,-5.6,4.5));
#8725=CARTESIAN_POINT('Origin',(0.,-5.,4.5));
#8726=CARTESIAN_POINT('Origin',(0.5,-6.7,3.4));
#8727=CARTESIAN_POINT('',(0.5,-5.6,5.5));
#8728=CARTESIAN_POINT('',(0.5,-6.6,5.5));
#8729=CARTESIAN_POINT('',(0.5,-6.25,5.5));
#8730=CARTESIAN_POINT('',(0.5,-5.6,3.5));
#8731=CARTESIAN_POINT('',(0.5,-5.6,3.4));
#8732=CARTESIAN_POINT('',(0.5,-6.6,3.5));
#8733=CARTESIAN_POINT('',(0.5,-6.25,3.5));
#8734=CARTESIAN_POINT('',(0.5,-6.6,3.45));
#8735=CARTESIAN_POINT('Origin',(0.5,-5.6,3.4));
#8736=CARTESIAN_POINT('',(-0.5,-5.6,5.5));
#8737=CARTESIAN_POINT('',(0.25,-5.6,5.5));
#8738=CARTESIAN_POINT('',(-0.5,-5.6,3.5));
#8739=CARTESIAN_POINT('',(-0.5,-5.6,3.4));
#8740=CARTESIAN_POINT('',(0.25,-5.6,3.5));
#8741=CARTESIAN_POINT('Origin',(-0.5,-5.6,3.4));
#8742=CARTESIAN_POINT('',(-0.5,-6.6,5.5));
#8743=CARTESIAN_POINT('',(-0.5,-5.7,5.5));
#8744=CARTESIAN_POINT('',(-0.5,-6.6,3.5));
#8745=CARTESIAN_POINT('',(-0.5,-6.6,3.45));
#8746=CARTESIAN_POINT('',(-0.5,-5.7,3.5));
#8747=CARTESIAN_POINT('Origin',(0.,-5.8,3.5));
#8748=CARTESIAN_POINT('',(-1.,-6.6,3.5));
#8749=CARTESIAN_POINT('',(-1.,-6.6,3.5));
#8750=CARTESIAN_POINT('',(-1.,-5.,3.5));
#8751=CARTESIAN_POINT('',(-1.,-5.,3.5));
#8752=CARTESIAN_POINT('',(1.,-5.,3.5));
#8753=CARTESIAN_POINT('',(1.,-5.,3.5));
#8754=CARTESIAN_POINT('',(1.,-6.6,3.5));
#8755=CARTESIAN_POINT('',(1.,-6.6,3.5));
#8756=CARTESIAN_POINT('',(-1.,-6.6,3.5));
#8757=CARTESIAN_POINT('Origin',(-1.,-6.6,3.5));
#8758=CARTESIAN_POINT('',(-1.,-6.6,5.5));
#8759=CARTESIAN_POINT('',(-1.,-6.6,5.5));
#8760=CARTESIAN_POINT('',(-1.,-6.6,3.5));
#8761=CARTESIAN_POINT('Origin',(-1.,-6.6,3.5));
#8762=CARTESIAN_POINT('',(1.,-6.6,5.5));
#8763=CARTESIAN_POINT('',(1.,-6.6,3.5));
#8764=CARTESIAN_POINT('',(-1.,-6.6,5.5));
#8765=CARTESIAN_POINT('Origin',(1.,-5.,3.5));
#8766=CARTESIAN_POINT('',(-1.,-5.,5.5));
#8767=CARTESIAN_POINT('',(-1.,-5.,3.5));
#8768=CARTESIAN_POINT('',(1.,-5.,5.5));
#8769=CARTESIAN_POINT('',(1.,-5.,5.5));
#8770=CARTESIAN_POINT('',(1.,-5.,3.5));
#8771=CARTESIAN_POINT('Origin',(1.,-6.6,3.5));
#8772=CARTESIAN_POINT('',(1.,-6.6,5.5));
#8773=CARTESIAN_POINT('Origin',(-1.,-5.,3.5));
#8774=CARTESIAN_POINT('',(-1.,-5.,5.5));
#8775=CARTESIAN_POINT('Origin',(0.,-5.8,5.5));
#8776=CARTESIAN_POINT('',(0.,0.,0.));
#8777=CARTESIAN_POINT('Origin',(0.0577350269189626,0.,-0.1));
#8778=CARTESIAN_POINT('',(0.0577350269189626,0.,-0.1));
#8779=CARTESIAN_POINT('',(0.115470053837925,0.,0.));
#8780=CARTESIAN_POINT('',(0.0934187836487032,0.,-0.0381939203391614));
#8781=CARTESIAN_POINT('',(0.0577350269189626,-0.2,-0.1));
#8782=CARTESIAN_POINT('',(0.0577350269189626,0.,-0.1));
#8783=CARTESIAN_POINT('',(0.115470053837925,-0.2,0.));
#8784=CARTESIAN_POINT('',(0.115470053837925,-0.2,0.));
#8785=CARTESIAN_POINT('',(0.115470053837925,0.,0.));
#8786=CARTESIAN_POINT('Origin',(-0.0577350269189626,0.,-0.1));
#8787=CARTESIAN_POINT('',(-0.0577350269189626,0.,-0.1));
#8788=CARTESIAN_POINT('',(0.0561324865405187,0.,-0.1));
#8789=CARTESIAN_POINT('',(-0.0577350269189626,-0.2,-0.1));
#8790=CARTESIAN_POINT('',(-0.0577350269189626,0.,-0.1));
#8791=CARTESIAN_POINT('',(0.0577350269189626,-0.2,-0.1));
#8792=CARTESIAN_POINT('Origin',(-0.115470053837925,0.,-1.38777878078145E-17));
#8793=CARTESIAN_POINT('',(-0.115470053837925,0.,-1.41410031829988E-17));
#8794=CARTESIAN_POINT('',(-0.0797862971081845,0.,-0.0618060796608387));
#8795=CARTESIAN_POINT('',(-0.115470053837925,-0.2,-1.38777878078145E-17));
#8796=CARTESIAN_POINT('',(-0.115470053837925,0.,-1.41410031829988E-17));
#8797=CARTESIAN_POINT('',(-0.0577350269189626,-0.2,-0.1));
#8798=CARTESIAN_POINT('Origin',(-0.0577350269189626,0.,0.1));
#8799=CARTESIAN_POINT('',(-0.0577350269189626,0.,0.1));
#8800=CARTESIAN_POINT('',(-0.0509187836487033,0.,0.111806079660839));
#8801=CARTESIAN_POINT('',(-0.0577350269189626,-0.2,0.1));
#8802=CARTESIAN_POINT('',(-0.0577350269189626,0.,0.1));
#8803=CARTESIAN_POINT('',(-0.115470053837925,-0.2,-1.41410031829988E-17));
#8804=CARTESIAN_POINT('Origin',(0.0577350269189626,0.,0.1));
#8805=CARTESIAN_POINT('',(0.0577350269189626,0.,0.1));
#8806=CARTESIAN_POINT('',(0.113867513459481,0.,0.1));
#8807=CARTESIAN_POINT('',(0.0577350269189626,-0.2,0.1));
#8808=CARTESIAN_POINT('',(0.0577350269189626,0.,0.1));
#8809=CARTESIAN_POINT('',(-0.0577350269189626,-0.2,0.1));
#8810=CARTESIAN_POINT('Origin',(0.115470053837925,0.,0.));
#8811=CARTESIAN_POINT('',(0.122286297108185,0.,-0.0118060796608386));
#8812=CARTESIAN_POINT('',(0.0577350269189626,-0.2,0.1));
#8813=CARTESIAN_POINT('Origin',(0.,-0.2,0.));
#8814=CARTESIAN_POINT('Origin',(0.17,0.,0.));
#8815=CARTESIAN_POINT('',(-0.17,-8.67361737988404E-18,-2.0818995585505E-17));
#8816=CARTESIAN_POINT('Origin',(0.,0.,0.));
#8817=CARTESIAN_POINT('Origin',(0.,-0.015,0.));
#8818=CARTESIAN_POINT('',(-0.1954,-0.0254,-2.39295984553393E-17));
#8819=CARTESIAN_POINT('Origin',(0.,-0.0254,0.));
#8820=CARTESIAN_POINT('',(-0.185,-0.015,-2.2655965784226E-17));
#8821=CARTESIAN_POINT('Origin',(0.,-0.2775,0.));
#8822=CARTESIAN_POINT('',(-0.1954,-0.5296,2.39295984553393E-17));
#8823=CARTESIAN_POINT('Origin',(0.,-0.5296,0.));
#8824=CARTESIAN_POINT('',(-0.1954,-0.2775,-2.39295984553393E-17));
#8825=CARTESIAN_POINT('Origin',(0.,-0.5625,0.));
#8826=CARTESIAN_POINT('',(-0.125,-0.6,-1.53080849893419E-17));
#8827=CARTESIAN_POINT('Origin',(0.,-0.6,0.));
#8828=CARTESIAN_POINT('',(-0.1625,-0.5625,-1.99005104861445E-17));
#8829=CARTESIAN_POINT('Origin',(0.,-0.6,0.));
#8830=CARTESIAN_POINT('',(0.,0.,0.));
#8831=CARTESIAN_POINT('Origin',(0.,-2.7,0.));
#8832=CARTESIAN_POINT('',(-0.289136645896019,-2.7,0.08));
#8833=CARTESIAN_POINT('',(-0.3,-2.78,-2.27065106771523E-17));
#8834=CARTESIAN_POINT('Ctrl Pts',(-0.289136645896019,-2.7,0.08));
#8835=CARTESIAN_POINT('Ctrl Pts',(-0.289136645896019,-2.71009877520201,
0.08));
#8836=CARTESIAN_POINT('Ctrl Pts',(-0.289720927595908,-2.72083518625944,
0.0779717130936404));
#8837=CARTESIAN_POINT('Ctrl Pts',(-0.291799203044223,-2.74052980652726,
0.0697927537456149));
#8838=CARTESIAN_POINT('Ctrl Pts',(-0.293259762986909,-2.74949254880105,
0.0636445361887959));
#8839=CARTESIAN_POINT('Ctrl Pts',(-0.295976783522942,-2.76364324458222,
0.0494938404076284));
#8840=CARTESIAN_POINT('Ctrl Pts',(-0.297414335384467,-2.76979246713824,
0.0405305642602551));
#8841=CARTESIAN_POINT('Ctrl Pts',(-0.299439403644655,-2.77797216257078,
0.0208340363410407));
#8842=CARTESIAN_POINT('Ctrl Pts',(-0.3,-2.78,0.0100969318362556));
#8843=CARTESIAN_POINT('Ctrl Pts',(-0.3,-2.78,5.20417042793042E-18));
#8844=CARTESIAN_POINT('',(0.289136645896019,-2.7,0.08));
#8845=CARTESIAN_POINT('',(0.,-2.7,0.08));
#8846=CARTESIAN_POINT('Ctrl Pts',(0.289136645896019,-2.7,0.08));
#8847=CARTESIAN_POINT('Ctrl Pts',(0.289136645896019,-2.68990122479799,0.08));
#8848=CARTESIAN_POINT('Ctrl Pts',(0.289720927595908,-2.67916481374056,0.0779717130936404));
#8849=CARTESIAN_POINT('Ctrl Pts',(0.291799203044223,-2.65947019347274,0.0697927537456147));
#8850=CARTESIAN_POINT('Ctrl Pts',(0.293259762986909,-2.65050745119895,0.0636445361887959));
#8851=CARTESIAN_POINT('Ctrl Pts',(0.295976783522942,-2.63635675541778,0.0494938404076283));
#8852=CARTESIAN_POINT('Ctrl Pts',(0.297414335384467,-2.63020753286176,0.0405305642602551));
#8853=CARTESIAN_POINT('Ctrl Pts',(0.299439403644655,-2.62202783742922,0.0208340363410406));
#8854=CARTESIAN_POINT('Ctrl Pts',(0.3,-2.62,0.0100969318362555));
#8855=CARTESIAN_POINT('Ctrl Pts',(0.3,-2.62,-0.0100969318362556));
#8856=CARTESIAN_POINT('Ctrl Pts',(0.299439403644655,-2.62202783742922,-0.0208340363410406));
#8857=CARTESIAN_POINT('Ctrl Pts',(0.297414335384467,-2.63020753286176,-0.0405305642602551));
#8858=CARTESIAN_POINT('Ctrl Pts',(0.295976783522942,-2.63635675541778,-0.0494938404076283));
#8859=CARTESIAN_POINT('Ctrl Pts',(0.293259762986909,-2.65050745119895,-0.0636445361887959));
#8860=CARTESIAN_POINT('Ctrl Pts',(0.291799203044223,-2.65947019347274,-0.0697927537456147));
#8861=CARTESIAN_POINT('Ctrl Pts',(0.289720927595908,-2.67916481374056,-0.0779717130936403));
#8862=CARTESIAN_POINT('Ctrl Pts',(0.289136645896019,-2.68990122479799,-0.08));
#8863=CARTESIAN_POINT('Ctrl Pts',(0.289136645896019,-2.71009877520201,-0.08));
#8864=CARTESIAN_POINT('Ctrl Pts',(0.289720927595908,-2.72083518625944,-0.0779717130936404));
#8865=CARTESIAN_POINT('Ctrl Pts',(0.291799203044223,-2.74052980652726,-0.0697927537456147));
#8866=CARTESIAN_POINT('Ctrl Pts',(0.293259762986909,-2.74949254880105,-0.0636445361887959));
#8867=CARTESIAN_POINT('Ctrl Pts',(0.295976783522942,-2.76364324458222,-0.0494938404076283));
#8868=CARTESIAN_POINT('Ctrl Pts',(0.297414335384467,-2.76979246713824,-0.0405305642602551));
#8869=CARTESIAN_POINT('Ctrl Pts',(0.299439403644655,-2.77797216257078,-0.0208340363410406));
#8870=CARTESIAN_POINT('Ctrl Pts',(0.3,-2.78,-0.0100969318362555));
#8871=CARTESIAN_POINT('Ctrl Pts',(0.3,-2.78,0.0100969318362556));
#8872=CARTESIAN_POINT('Ctrl Pts',(0.299439403644655,-2.77797216257078,0.0208340363410407));
#8873=CARTESIAN_POINT('Ctrl Pts',(0.297414335384467,-2.76979246713824,0.0405305642602551));
#8874=CARTESIAN_POINT('Ctrl Pts',(0.295976783522942,-2.76364324458222,0.0494938404076284));
#8875=CARTESIAN_POINT('Ctrl Pts',(0.293259762986909,-2.74949254880105,0.0636445361887959));
#8876=CARTESIAN_POINT('Ctrl Pts',(0.291799203044223,-2.74052980652726,0.0697927537456149));
#8877=CARTESIAN_POINT('Ctrl Pts',(0.289720927595908,-2.72083518625944,0.0779717130936404));
#8878=CARTESIAN_POINT('Ctrl Pts',(0.289136645896019,-2.71009877520201,0.08));
#8879=CARTESIAN_POINT('Ctrl Pts',(0.289136645896019,-2.7,0.08));
#8880=CARTESIAN_POINT('',(-0.3,-2.62,-3.65842984849668E-17));
#8881=CARTESIAN_POINT('Ctrl Pts',(-0.3,-2.62,-3.81639164714898E-17));
#8882=CARTESIAN_POINT('Ctrl Pts',(-0.3,-2.62,0.0100969318362555));
#8883=CARTESIAN_POINT('Ctrl Pts',(-0.299439403644655,-2.62202783742922,
0.0208340363410406));
#8884=CARTESIAN_POINT('Ctrl Pts',(-0.297414335384467,-2.63020753286176,
0.040530564260255));
#8885=CARTESIAN_POINT('Ctrl Pts',(-0.295976783522942,-2.63635675541778,
0.0494938404076283));
#8886=CARTESIAN_POINT('Ctrl Pts',(-0.293259762986909,-2.65050745119895,
0.0636445361887959));
#8887=CARTESIAN_POINT('Ctrl Pts',(-0.291799203044223,-2.65947019347274,
0.0697927537456147));
#8888=CARTESIAN_POINT('Ctrl Pts',(-0.289720927595908,-2.67916481374056,
0.0779717130936404));
#8889=CARTESIAN_POINT('Ctrl Pts',(-0.289136645896019,-2.68990122479799,
0.08));
#8890=CARTESIAN_POINT('Ctrl Pts',(-0.289136645896019,-2.7,0.08));
#8891=CARTESIAN_POINT('Ctrl Pts',(-0.3,-2.78,-6.93889390390723E-18));
#8892=CARTESIAN_POINT('Ctrl Pts',(-0.3,-2.78,-0.0100969318362556));
#8893=CARTESIAN_POINT('Ctrl Pts',(-0.299439403644655,-2.77797216257078,
-0.0208340363410406));
#8894=CARTESIAN_POINT('Ctrl Pts',(-0.297414335384467,-2.76979246713824,
-0.0405305642602551));
#8895=CARTESIAN_POINT('Ctrl Pts',(-0.295976783522942,-2.76364324458222,
-0.0494938404076283));
#8896=CARTESIAN_POINT('Ctrl Pts',(-0.293259762986909,-2.74949254880105,
-0.0636445361887959));
#8897=CARTESIAN_POINT('Ctrl Pts',(-0.291799203044223,-2.74052980652726,
-0.0697927537456147));
#8898=CARTESIAN_POINT('Ctrl Pts',(-0.289720927595908,-2.72083518625944,
-0.0779717130936403));
#8899=CARTESIAN_POINT('Ctrl Pts',(-0.289136645896019,-2.71009877520201,
-0.08));
#8900=CARTESIAN_POINT('Ctrl Pts',(-0.289136645896019,-2.68990122479799,
-0.08));
#8901=CARTESIAN_POINT('Ctrl Pts',(-0.289720927595908,-2.67916481374056,
-0.0779717130936403));
#8902=CARTESIAN_POINT('Ctrl Pts',(-0.291799203044223,-2.65947019347274,
-0.0697927537456147));
#8903=CARTESIAN_POINT('Ctrl Pts',(-0.293259762986909,-2.65050745119895,
-0.0636445361887959));
#8904=CARTESIAN_POINT('Ctrl Pts',(-0.295976783522942,-2.63635675541778,
-0.0494938404076283));
#8905=CARTESIAN_POINT('Ctrl Pts',(-0.297414335384467,-2.63020753286176,
-0.0405305642602551));
#8906=CARTESIAN_POINT('Ctrl Pts',(-0.299439403644655,-2.62202783742922,
-0.0208340363410406));
#8907=CARTESIAN_POINT('Ctrl Pts',(-0.3,-2.62,-0.0100969318362556));
#8908=CARTESIAN_POINT('Ctrl Pts',(-0.3,-2.62,-1.56125112837913E-17));
#8909=CARTESIAN_POINT('Origin',(0.45,0.2,0.));
#8910=CARTESIAN_POINT('',(-0.45,0.2,-5.51091059616309E-17));
#8911=CARTESIAN_POINT('Origin',(0.,0.2,0.));
#8912=CARTESIAN_POINT('Origin',(0.,0.175,0.));
#8913=CARTESIAN_POINT('',(-0.5,0.15,-6.12323399573676E-17));
#8914=CARTESIAN_POINT('Origin',(0.,0.15,0.));
#8915=CARTESIAN_POINT('',(-0.475,0.175,-5.81707229594993E-17));
#8916=CARTESIAN_POINT('Origin',(0.,0.0750000000000002,0.));
#8917=CARTESIAN_POINT('',(-0.5,0.,-6.12323399573677E-17));
#8918=CARTESIAN_POINT('Origin',(0.,0.,0.));
#8919=CARTESIAN_POINT('',(-0.5,0.0750000000000002,-6.12323399573677E-17));
#8920=CARTESIAN_POINT('Origin',(0.3,0.,0.));
#8921=CARTESIAN_POINT('',(-0.3,0.,-3.67394039744206E-17));
#8922=CARTESIAN_POINT('Origin',(0.,0.,0.));
#8923=CARTESIAN_POINT('Origin',(0.,-1.455,0.));
#8924=CARTESIAN_POINT('',(-0.3,-2.91,-3.67394039744206E-17));
#8925=CARTESIAN_POINT('Origin',(0.,-2.91,0.));
#8926=CARTESIAN_POINT('',(-0.3,-1.455,-3.67394039744206E-17));
#8927=CARTESIAN_POINT('',(-0.3,-1.455,-3.67394039744206E-17));
#8928=CARTESIAN_POINT('Origin',(0.,-2.955,0.));
#8929=CARTESIAN_POINT('',(-0.21,-3.,-2.57175827820944E-17));
#8930=CARTESIAN_POINT('Origin',(0.,-3.,0.));
#8931=CARTESIAN_POINT('',(-0.255,-2.955,-3.12284933782575E-17));
#8932=CARTESIAN_POINT('Origin',(0.,-3.,0.));
#8933=CARTESIAN_POINT('',(0.,0.,0.));
#8934=CARTESIAN_POINT('Origin',(0.,0.,0.));
#8935=CARTESIAN_POINT('',(-0.32,0.16,3.91886975727153E-17));
#8936=CARTESIAN_POINT('Origin',(0.,0.16,0.));
#8937=CARTESIAN_POINT('',(-0.32,0.,3.91886975727153E-17));
#8938=CARTESIAN_POINT('',(-0.32,0.,3.91886975727153E-17));
#8939=CARTESIAN_POINT('Origin',(0.,0.,0.));
#8940=CARTESIAN_POINT('Origin',(0.,0.,0.));
#8941=CARTESIAN_POINT('',(-0.6,0.16,7.34788079488412E-17));
#8942=CARTESIAN_POINT('Origin',(0.,0.16,0.));
#8943=CARTESIAN_POINT('',(-0.6,0.,7.34788079488412E-17));
#8944=CARTESIAN_POINT('',(-0.6,0.,7.34788079488412E-17));
#8945=CARTESIAN_POINT('Origin',(0.,0.,0.));
#8946=CARTESIAN_POINT('Origin',(0.,0.16,0.));
#8947=CARTESIAN_POINT('Origin',(0.,0.,0.));
#8948=CARTESIAN_POINT('',(0.,0.,0.));
#8949=CARTESIAN_POINT('Origin',(0.,0.12,0.));
#8950=CARTESIAN_POINT('',(-9.79717439317883E-18,0.12,-0.04));
#8951=CARTESIAN_POINT('Origin',(0.,0.12,-0.12));
#8952=CARTESIAN_POINT('Origin',(9.79717439317883E-18,0.12,0.));
#8953=CARTESIAN_POINT('',(0.08,-4.89858719658941E-18,7.34788079488412E-18));
#8954=CARTESIAN_POINT('',(-0.08,-4.89858719658941E-18,7.34788079488412E-18));
#8955=CARTESIAN_POINT('Ctrl Pts',(0.08,-4.89858719658941E-18,7.34788079488412E-18));
#8956=CARTESIAN_POINT('Ctrl Pts',(0.08,-0.00012864962353541,0.000128649623535413));
#8957=CARTESIAN_POINT('Ctrl Pts',(0.0799996896739287,-0.00025719571182076,
0.000257402596003253));
#8958=CARTESIAN_POINT('Ctrl Pts',(0.0799669711262291,-0.00701193164572964,
0.00703384588894362));
#8959=CARTESIAN_POINT('Ctrl Pts',(0.0791054994909294,-0.0133457972655825,
0.0139383126556792));
#8960=CARTESIAN_POINT('Ctrl Pts',(0.0749700088488058,-0.0265076530862524,
0.0292212026164895));
#8961=CARTESIAN_POINT('Ctrl Pts',(0.0712702072865517,-0.0331317062461458,
0.0375603420117568));
#8962=CARTESIAN_POINT('Ctrl Pts',(0.0612858949407667,-0.0440683985740427,
0.0520545604187517));
#8963=CARTESIAN_POINT('Ctrl Pts',(0.0555090276731744,-0.0485199197794574,
0.0582717815295611));
#8964=CARTESIAN_POINT('Ctrl Pts',(0.0412398082144208,-0.0561090538733877,
0.0691638397919718));
#8965=CARTESIAN_POINT('Ctrl Pts',(0.0327878980890048,-0.059089642483296,
0.0736229049587921));
#8966=CARTESIAN_POINT('Ctrl Pts',(0.0159233027310102,-0.0625179833270725,
0.0787936360751706));
#8967=CARTESIAN_POINT('Ctrl Pts',(0.00801661414593076,-0.0633030277982336,
0.08));
#8968=CARTESIAN_POINT('Ctrl Pts',(-0.00801661414593074,-0.0633030277982336,
0.08));
#8969=CARTESIAN_POINT('Ctrl Pts',(-0.0159233027310102,-0.0625179833270726,
0.0787936360751706));
#8970=CARTESIAN_POINT('Ctrl Pts',(-0.0327878980890049,-0.059089642483296,
0.0736229049587921));
#8971=CARTESIAN_POINT('Ctrl Pts',(-0.0412398082144209,-0.0561090538733877,
0.0691638397919717));
#8972=CARTESIAN_POINT('Ctrl Pts',(-0.0555090276731744,-0.0485199197794574,
0.0582717815295611));
#8973=CARTESIAN_POINT('Ctrl Pts',(-0.0612858949407667,-0.0440683985740427,
0.0520545604187517));
#8974=CARTESIAN_POINT('Ctrl Pts',(-0.0712702072865517,-0.0331317062461458,
0.0375603420117568));
#8975=CARTESIAN_POINT('Ctrl Pts',(-0.0749700088488058,-0.0265076530862524,
0.0292212026164895));
#8976=CARTESIAN_POINT('Ctrl Pts',(-0.0791054994909264,-0.0133457972655921,
0.0139383126556903));
#8977=CARTESIAN_POINT('Ctrl Pts',(-0.0799669711262287,-0.00701193164579759,
0.0070338458890125));
#8978=CARTESIAN_POINT('Ctrl Pts',(-0.0799996896739287,-0.000257195711817665,
0.000257402596000083));
#8979=CARTESIAN_POINT('Ctrl Pts',(-0.08,-0.000128649623538514,0.000128649623538516));
#8980=CARTESIAN_POINT('Ctrl Pts',(-0.08,-4.89858719658941E-18,7.34788079488412E-18));
#8981=CARTESIAN_POINT('Ctrl Pts',(-0.08,-4.89858719658941E-18,7.34788079488412E-18));
#8982=CARTESIAN_POINT('Ctrl Pts',(-0.08,-0.000128649623536042,-0.00012864962353603));
#8983=CARTESIAN_POINT('Ctrl Pts',(-0.0799996896739287,-0.000257195711820127,
-0.000257402596002604));
#8984=CARTESIAN_POINT('Ctrl Pts',(-0.0799669711262289,-0.0070119316457589,
-0.00703384588897312));
#8985=CARTESIAN_POINT('Ctrl Pts',(-0.0791054994909281,-0.0133457972655867,
-0.0139383126556841));
#8986=CARTESIAN_POINT('Ctrl Pts',(-0.0749700088488058,-0.0265076530862525,
-0.0292212026164896));
#8987=CARTESIAN_POINT('Ctrl Pts',(-0.0712702072865516,-0.0331317062461459,
-0.0375603420117568));
#8988=CARTESIAN_POINT('Ctrl Pts',(-0.0612858949407667,-0.0440683985740427,
-0.0520545604187517));
#8989=CARTESIAN_POINT('Ctrl Pts',(-0.0555090276731744,-0.0485199197794574,
-0.0582717815295611));
#8990=CARTESIAN_POINT('Ctrl Pts',(-0.0412398082144209,-0.0561090538733877,
-0.0691638397919717));
#8991=CARTESIAN_POINT('Ctrl Pts',(-0.0327878980890049,-0.059089642483296,
-0.0736229049587921));
#8992=CARTESIAN_POINT('Ctrl Pts',(-0.0159233027310101,-0.0625179833270725,
-0.0787936360751706));
#8993=CARTESIAN_POINT('Ctrl Pts',(-0.00801661414593069,-0.0633030277982336,
-0.08));
#8994=CARTESIAN_POINT('Ctrl Pts',(0.0080166141459307,-0.0633030277982336,
-0.08));
#8995=CARTESIAN_POINT('Ctrl Pts',(0.0159233027310101,-0.0625179833270725,
-0.0787936360751706));
#8996=CARTESIAN_POINT('Ctrl Pts',(0.0327878980890049,-0.0590896424832959,
-0.0736229049587921));
#8997=CARTESIAN_POINT('Ctrl Pts',(0.0412398082144209,-0.0561090538733877,
-0.0691638397919717));
#8998=CARTESIAN_POINT('Ctrl Pts',(0.0555090276731744,-0.0485199197794574,
-0.0582717815295611));
#8999=CARTESIAN_POINT('Ctrl Pts',(0.0612858949407666,-0.0440683985740428,
-0.0520545604187518));
#9000=CARTESIAN_POINT('Ctrl Pts',(0.0712702072865517,-0.0331317062461458,
-0.0375603420117568));
#9001=CARTESIAN_POINT('Ctrl Pts',(0.0749700088488058,-0.0265076530862524,
-0.0292212026164895));
#9002=CARTESIAN_POINT('Ctrl Pts',(0.079105499490928,-0.013345797265587,
-0.0139383126556845));
#9003=CARTESIAN_POINT('Ctrl Pts',(0.0799669711262289,-0.00701193164576148,
-0.00703384588897579));
#9004=CARTESIAN_POINT('Ctrl Pts',(0.0799996896739287,-0.000257195711819584,
-0.000257402596002039));
#9005=CARTESIAN_POINT('Ctrl Pts',(0.08,-0.000128649623536605,-0.000128649623536593));
#9006=CARTESIAN_POINT('Ctrl Pts',(0.08,-4.89858719658941E-18,7.34788079488412E-18));
#9007=CARTESIAN_POINT('Origin',(0.04,-1.36,0.));
#9008=CARTESIAN_POINT('',(0.,-1.36,-0.08));
#9009=CARTESIAN_POINT('',(0.,-1.36,0.08));
#9010=CARTESIAN_POINT('Origin',(0.,-1.36,0.));
#9011=CARTESIAN_POINT('',(0.,-1.36,-0.04));
#9012=CARTESIAN_POINT('Origin',(0.,0.,-0.08));
#9013=CARTESIAN_POINT('',(0.,-1.6,0.08));
#9014=CARTESIAN_POINT('',(0.,0.,0.08));
#9015=CARTESIAN_POINT('',(0.,-1.6,-0.08));
#9016=CARTESIAN_POINT('',(0.,-1.6,-0.09));
#9017=CARTESIAN_POINT('',(0.,0.,-0.08));
#9018=CARTESIAN_POINT('Origin',(0.,0.,0.));
#9019=CARTESIAN_POINT('',(-0.08,-1.6,-9.79717439317883E-18));
#9020=CARTESIAN_POINT('Origin',(0.,-1.6,0.));
#9021=CARTESIAN_POINT('',(-0.08,0.,-9.79717439317883E-18));
#9022=CARTESIAN_POINT('Origin',(0.,-1.6,0.));
#9023=CARTESIAN_POINT('Origin',(-0.04,-1.6,0.));
#9024=CARTESIAN_POINT('',(0.,0.,0.));
#9025=CARTESIAN_POINT('',(0.,0.,0.));
#9026=CARTESIAN_POINT('',(0.,0.,0.));
#9027=CARTESIAN_POINT('',(0.,3.2,4.5));
#9028=CARTESIAN_POINT('',(0.,0.,0.));
#9029=CARTESIAN_POINT('',(0.,-5.3,5.5));
#9030=CARTESIAN_POINT('',(-1.16,-6.1,4.5));
#9031=CARTESIAN_POINT('',(-1.16,-6.1,4.5));
#9032=CARTESIAN_POINT('',(1.,-6.1,4.5));
#9033=CARTESIAN_POINT('',(1.16,-6.1,4.5));
#9034=CARTESIAN_POINT('',(1.54,-5.7,4.5));
#9035=CARTESIAN_POINT('',(0.,0.,0.));
#9036=CARTESIAN_POINT('',(0.,0.,0.));
#9037=UNCERTAINTY_MEASURE_WITH_UNIT(LENGTH_MEASURE(0.001),#9103,
'DISTANCE_ACCURACY_VALUE',
'Maximum model space distance between geometric entities at asserted c
onnectivities');
#9038=UNCERTAINTY_MEASURE_WITH_UNIT(LENGTH_MEASURE(0.001),#9103,
'DISTANCE_ACCURACY_VALUE',
'Maximum model space distance between geometric entities at asserted c
onnectivities');
#9039=UNCERTAINTY_MEASURE_WITH_UNIT(LENGTH_MEASURE(0.001),#9103,
'DISTANCE_ACCURACY_VALUE',
'Maximum model space distance between geometric entities at asserted c
onnectivities');
#9040=UNCERTAINTY_MEASURE_WITH_UNIT(LENGTH_MEASURE(0.001),#9103,
'DISTANCE_ACCURACY_VALUE',
'Maximum model space distance between geometric entities at asserted c
onnectivities');
#9041=UNCERTAINTY_MEASURE_WITH_UNIT(LENGTH_MEASURE(0.001),#9103,
'DISTANCE_ACCURACY_VALUE',
'Maximum model space distance between geometric entities at asserted c
onnectivities');
#9042=UNCERTAINTY_MEASURE_WITH_UNIT(LENGTH_MEASURE(0.001),#9103,
'DISTANCE_ACCURACY_VALUE',
'Maximum model space distance between geometric entities at asserted c
onnectivities');
#9043=UNCERTAINTY_MEASURE_WITH_UNIT(LENGTH_MEASURE(0.001),#9103,
'DISTANCE_ACCURACY_VALUE',
'Maximum model space distance between geometric entities at asserted c
onnectivities');
#9044=UNCERTAINTY_MEASURE_WITH_UNIT(LENGTH_MEASURE(0.001),#9103,
'DISTANCE_ACCURACY_VALUE',
'Maximum model space distance between geometric entities at asserted c
onnectivities');
#9045=UNCERTAINTY_MEASURE_WITH_UNIT(LENGTH_MEASURE(0.001),#9103,
'DISTANCE_ACCURACY_VALUE',
'Maximum model space distance between geometric entities at asserted c
onnectivities');
#9046=UNCERTAINTY_MEASURE_WITH_UNIT(LENGTH_MEASURE(0.001),#9103,
'DISTANCE_ACCURACY_VALUE',
'Maximum model space distance between geometric entities at asserted c
onnectivities');
#9047=UNCERTAINTY_MEASURE_WITH_UNIT(LENGTH_MEASURE(0.001),#9103,
'DISTANCE_ACCURACY_VALUE',
'Maximum model space distance between geometric entities at asserted c
onnectivities');
#9048=UNCERTAINTY_MEASURE_WITH_UNIT(LENGTH_MEASURE(0.001),#9103,
'DISTANCE_ACCURACY_VALUE',
'Maximum model space distance between geometric entities at asserted c
onnectivities');
#9049=UNCERTAINTY_MEASURE_WITH_UNIT(LENGTH_MEASURE(0.001),#9103,
'DISTANCE_ACCURACY_VALUE',
'Maximum model space distance between geometric entities at asserted c
onnectivities');
#9050=UNCERTAINTY_MEASURE_WITH_UNIT(LENGTH_MEASURE(0.001),#9103,
'DISTANCE_ACCURACY_VALUE',
'Maximum model space distance between geometric entities at asserted c
onnectivities');
#9051=UNCERTAINTY_MEASURE_WITH_UNIT(LENGTH_MEASURE(0.001),#9103,
'DISTANCE_ACCURACY_VALUE',
'Maximum model space distance between geometric entities at asserted c
onnectivities');
#9052=UNCERTAINTY_MEASURE_WITH_UNIT(LENGTH_MEASURE(0.001),#9103,
'DISTANCE_ACCURACY_VALUE',
'Maximum model space distance between geometric entities at asserted c
onnectivities');
#9053=UNCERTAINTY_MEASURE_WITH_UNIT(LENGTH_MEASURE(0.001),#9103,
'DISTANCE_ACCURACY_VALUE',
'Maximum model space distance between geometric entities at asserted c
onnectivities');
#9054=UNCERTAINTY_MEASURE_WITH_UNIT(LENGTH_MEASURE(0.001),#9103,
'DISTANCE_ACCURACY_VALUE',
'Maximum model space distance between geometric entities at asserted c
onnectivities');
#9055=UNCERTAINTY_MEASURE_WITH_UNIT(LENGTH_MEASURE(0.001),#9103,
'DISTANCE_ACCURACY_VALUE',
'Maximum model space distance between geometric entities at asserted c
onnectivities');
#9056=UNCERTAINTY_MEASURE_WITH_UNIT(LENGTH_MEASURE(0.001),#9103,
'DISTANCE_ACCURACY_VALUE',
'Maximum model space distance between geometric entities at asserted c
onnectivities');
#9057=UNCERTAINTY_MEASURE_WITH_UNIT(LENGTH_MEASURE(0.001),#9103,
'DISTANCE_ACCURACY_VALUE',
'Maximum model space distance between geometric entities at asserted c
onnectivities');
#9058=UNCERTAINTY_MEASURE_WITH_UNIT(LENGTH_MEASURE(0.001),#9103,
'DISTANCE_ACCURACY_VALUE',
'Maximum model space distance between geometric entities at asserted c
onnectivities');
#9059=UNCERTAINTY_MEASURE_WITH_UNIT(LENGTH_MEASURE(0.001),#9103,
'DISTANCE_ACCURACY_VALUE',
'Maximum model space distance between geometric entities at asserted c
onnectivities');
#9060=UNCERTAINTY_MEASURE_WITH_UNIT(LENGTH_MEASURE(0.001),#9103,
'DISTANCE_ACCURACY_VALUE',
'Maximum model space distance between geometric entities at asserted c
onnectivities');
#9061=UNCERTAINTY_MEASURE_WITH_UNIT(LENGTH_MEASURE(0.001),#9103,
'DISTANCE_ACCURACY_VALUE',
'Maximum model space distance between geometric entities at asserted c
onnectivities');
#9062=UNCERTAINTY_MEASURE_WITH_UNIT(LENGTH_MEASURE(0.001),#9103,
'DISTANCE_ACCURACY_VALUE',
'Maximum model space distance between geometric entities at asserted c
onnectivities');
#9063=UNCERTAINTY_MEASURE_WITH_UNIT(LENGTH_MEASURE(0.001),#9103,
'DISTANCE_ACCURACY_VALUE',
'Maximum model space distance between geometric entities at asserted c
onnectivities');
#9064=UNCERTAINTY_MEASURE_WITH_UNIT(LENGTH_MEASURE(0.001),#9103,
'DISTANCE_ACCURACY_VALUE',
'Maximum model space distance between geometric entities at asserted c
onnectivities');
#9065=UNCERTAINTY_MEASURE_WITH_UNIT(LENGTH_MEASURE(0.001),#9103,
'DISTANCE_ACCURACY_VALUE',
'Maximum model space distance between geometric entities at asserted c
onnectivities');
#9066=UNCERTAINTY_MEASURE_WITH_UNIT(LENGTH_MEASURE(0.001),#9103,
'DISTANCE_ACCURACY_VALUE',
'Maximum model space distance between geometric entities at asserted c
onnectivities');
#9067=UNCERTAINTY_MEASURE_WITH_UNIT(LENGTH_MEASURE(0.001),#9103,
'DISTANCE_ACCURACY_VALUE',
'Maximum model space distance between geometric entities at asserted c
onnectivities');
#9068=UNCERTAINTY_MEASURE_WITH_UNIT(LENGTH_MEASURE(0.001),#9103,
'DISTANCE_ACCURACY_VALUE',
'Maximum model space distance between geometric entities at asserted c
onnectivities');
#9069=UNCERTAINTY_MEASURE_WITH_UNIT(LENGTH_MEASURE(0.001),#9103,
'DISTANCE_ACCURACY_VALUE',
'Maximum model space distance between geometric entities at asserted c
onnectivities');
#9070=(
GEOMETRIC_REPRESENTATION_CONTEXT(3)
GLOBAL_UNCERTAINTY_ASSIGNED_CONTEXT((#9037))
GLOBAL_UNIT_ASSIGNED_CONTEXT((#9103,#9105,#9106))
REPRESENTATION_CONTEXT('','3D')
);
#9071=(
GEOMETRIC_REPRESENTATION_CONTEXT(3)
GLOBAL_UNCERTAINTY_ASSIGNED_CONTEXT((#9038))
GLOBAL_UNIT_ASSIGNED_CONTEXT((#9103,#9105,#9106))
REPRESENTATION_CONTEXT('','3D')
);
#9072=(
GEOMETRIC_REPRESENTATION_CONTEXT(3)
GLOBAL_UNCERTAINTY_ASSIGNED_CONTEXT((#9039))
GLOBAL_UNIT_ASSIGNED_CONTEXT((#9103,#9105,#9106))
REPRESENTATION_CONTEXT('','3D')
);
#9073=(
GEOMETRIC_REPRESENTATION_CONTEXT(3)
GLOBAL_UNCERTAINTY_ASSIGNED_CONTEXT((#9040))
GLOBAL_UNIT_ASSIGNED_CONTEXT((#9103,#9105,#9106))
REPRESENTATION_CONTEXT('','3D')
);
#9074=(
GEOMETRIC_REPRESENTATION_CONTEXT(3)
GLOBAL_UNCERTAINTY_ASSIGNED_CONTEXT((#9041))
GLOBAL_UNIT_ASSIGNED_CONTEXT((#9103,#9105,#9106))
REPRESENTATION_CONTEXT('','3D')
);
#9075=(
GEOMETRIC_REPRESENTATION_CONTEXT(3)
GLOBAL_UNCERTAINTY_ASSIGNED_CONTEXT((#9042))
GLOBAL_UNIT_ASSIGNED_CONTEXT((#9103,#9105,#9106))
REPRESENTATION_CONTEXT('','3D')
);
#9076=(
GEOMETRIC_REPRESENTATION_CONTEXT(3)
GLOBAL_UNCERTAINTY_ASSIGNED_CONTEXT((#9043))
GLOBAL_UNIT_ASSIGNED_CONTEXT((#9103,#9105,#9106))
REPRESENTATION_CONTEXT('','3D')
);
#9077=(
GEOMETRIC_REPRESENTATION_CONTEXT(3)
GLOBAL_UNCERTAINTY_ASSIGNED_CONTEXT((#9044))
GLOBAL_UNIT_ASSIGNED_CONTEXT((#9103,#9105,#9106))
REPRESENTATION_CONTEXT('','3D')
);
#9078=(
GEOMETRIC_REPRESENTATION_CONTEXT(3)
GLOBAL_UNCERTAINTY_ASSIGNED_CONTEXT((#9045))
GLOBAL_UNIT_ASSIGNED_CONTEXT((#9103,#9105,#9106))
REPRESENTATION_CONTEXT('','3D')
);
#9079=(
GEOMETRIC_REPRESENTATION_CONTEXT(3)
GLOBAL_UNCERTAINTY_ASSIGNED_CONTEXT((#9046))
GLOBAL_UNIT_ASSIGNED_CONTEXT((#9103,#9105,#9106))
REPRESENTATION_CONTEXT('','3D')
);
#9080=(
GEOMETRIC_REPRESENTATION_CONTEXT(3)
GLOBAL_UNCERTAINTY_ASSIGNED_CONTEXT((#9047))
GLOBAL_UNIT_ASSIGNED_CONTEXT((#9103,#9105,#9106))
REPRESENTATION_CONTEXT('','3D')
);
#9081=(
GEOMETRIC_REPRESENTATION_CONTEXT(3)
GLOBAL_UNCERTAINTY_ASSIGNED_CONTEXT((#9048))
GLOBAL_UNIT_ASSIGNED_CONTEXT((#9103,#9105,#9106))
REPRESENTATION_CONTEXT('','3D')
);
#9082=(
GEOMETRIC_REPRESENTATION_CONTEXT(3)
GLOBAL_UNCERTAINTY_ASSIGNED_CONTEXT((#9049))
GLOBAL_UNIT_ASSIGNED_CONTEXT((#9103,#9105,#9106))
REPRESENTATION_CONTEXT('','3D')
);
#9083=(
GEOMETRIC_REPRESENTATION_CONTEXT(3)
GLOBAL_UNCERTAINTY_ASSIGNED_CONTEXT((#9050))
GLOBAL_UNIT_ASSIGNED_CONTEXT((#9103,#9105,#9106))
REPRESENTATION_CONTEXT('','3D')
);
#9084=(
GEOMETRIC_REPRESENTATION_CONTEXT(3)
GLOBAL_UNCERTAINTY_ASSIGNED_CONTEXT((#9051))
GLOBAL_UNIT_ASSIGNED_CONTEXT((#9103,#9105,#9106))
REPRESENTATION_CONTEXT('','3D')
);
#9085=(
GEOMETRIC_REPRESENTATION_CONTEXT(3)
GLOBAL_UNCERTAINTY_ASSIGNED_CONTEXT((#9052))
GLOBAL_UNIT_ASSIGNED_CONTEXT((#9103,#9105,#9106))
REPRESENTATION_CONTEXT('','3D')
);
#9086=(
GEOMETRIC_REPRESENTATION_CONTEXT(3)
GLOBAL_UNCERTAINTY_ASSIGNED_CONTEXT((#9053))
GLOBAL_UNIT_ASSIGNED_CONTEXT((#9103,#9105,#9106))
REPRESENTATION_CONTEXT('','3D')
);
#9087=(
GEOMETRIC_REPRESENTATION_CONTEXT(3)
GLOBAL_UNCERTAINTY_ASSIGNED_CONTEXT((#9054))
GLOBAL_UNIT_ASSIGNED_CONTEXT((#9103,#9105,#9106))
REPRESENTATION_CONTEXT('','3D')
);
#9088=(
GEOMETRIC_REPRESENTATION_CONTEXT(3)
GLOBAL_UNCERTAINTY_ASSIGNED_CONTEXT((#9055))
GLOBAL_UNIT_ASSIGNED_CONTEXT((#9103,#9105,#9106))
REPRESENTATION_CONTEXT('','3D')
);
#9089=(
GEOMETRIC_REPRESENTATION_CONTEXT(3)
GLOBAL_UNCERTAINTY_ASSIGNED_CONTEXT((#9056))
GLOBAL_UNIT_ASSIGNED_CONTEXT((#9103,#9105,#9106))
REPRESENTATION_CONTEXT('','3D')
);
#9090=(
GEOMETRIC_REPRESENTATION_CONTEXT(3)
GLOBAL_UNCERTAINTY_ASSIGNED_CONTEXT((#9057))
GLOBAL_UNIT_ASSIGNED_CONTEXT((#9103,#9105,#9106))
REPRESENTATION_CONTEXT('','3D')
);
#9091=(
GEOMETRIC_REPRESENTATION_CONTEXT(3)
GLOBAL_UNCERTAINTY_ASSIGNED_CONTEXT((#9058))
GLOBAL_UNIT_ASSIGNED_CONTEXT((#9103,#9105,#9106))
REPRESENTATION_CONTEXT('','3D')
);
#9092=(
GEOMETRIC_REPRESENTATION_CONTEXT(3)
GLOBAL_UNCERTAINTY_ASSIGNED_CONTEXT((#9059))
GLOBAL_UNIT_ASSIGNED_CONTEXT((#9103,#9105,#9106))
REPRESENTATION_CONTEXT('','3D')
);
#9093=(
GEOMETRIC_REPRESENTATION_CONTEXT(3)
GLOBAL_UNCERTAINTY_ASSIGNED_CONTEXT((#9060))
GLOBAL_UNIT_ASSIGNED_CONTEXT((#9103,#9105,#9106))
REPRESENTATION_CONTEXT('','3D')
);
#9094=(
GEOMETRIC_REPRESENTATION_CONTEXT(3)
GLOBAL_UNCERTAINTY_ASSIGNED_CONTEXT((#9061))
GLOBAL_UNIT_ASSIGNED_CONTEXT((#9103,#9105,#9106))
REPRESENTATION_CONTEXT('','3D')
);
#9095=(
GEOMETRIC_REPRESENTATION_CONTEXT(3)
GLOBAL_UNCERTAINTY_ASSIGNED_CONTEXT((#9062))
GLOBAL_UNIT_ASSIGNED_CONTEXT((#9103,#9105,#9106))
REPRESENTATION_CONTEXT('','3D')
);
#9096=(
GEOMETRIC_REPRESENTATION_CONTEXT(3)
GLOBAL_UNCERTAINTY_ASSIGNED_CONTEXT((#9063))
GLOBAL_UNIT_ASSIGNED_CONTEXT((#9103,#9105,#9106))
REPRESENTATION_CONTEXT('','3D')
);
#9097=(
GEOMETRIC_REPRESENTATION_CONTEXT(3)
GLOBAL_UNCERTAINTY_ASSIGNED_CONTEXT((#9064))
GLOBAL_UNIT_ASSIGNED_CONTEXT((#9103,#9105,#9106))
REPRESENTATION_CONTEXT('','3D')
);
#9098=(
GEOMETRIC_REPRESENTATION_CONTEXT(3)
GLOBAL_UNCERTAINTY_ASSIGNED_CONTEXT((#9065))
GLOBAL_UNIT_ASSIGNED_CONTEXT((#9103,#9105,#9106))
REPRESENTATION_CONTEXT('','3D')
);
#9099=(
GEOMETRIC_REPRESENTATION_CONTEXT(3)
GLOBAL_UNCERTAINTY_ASSIGNED_CONTEXT((#9066))
GLOBAL_UNIT_ASSIGNED_CONTEXT((#9103,#9105,#9106))
REPRESENTATION_CONTEXT('','3D')
);
#9100=(
GEOMETRIC_REPRESENTATION_CONTEXT(3)
GLOBAL_UNCERTAINTY_ASSIGNED_CONTEXT((#9067))
GLOBAL_UNIT_ASSIGNED_CONTEXT((#9103,#9105,#9106))
REPRESENTATION_CONTEXT('','3D')
);
#9101=(
GEOMETRIC_REPRESENTATION_CONTEXT(3)
GLOBAL_UNCERTAINTY_ASSIGNED_CONTEXT((#9068))
GLOBAL_UNIT_ASSIGNED_CONTEXT((#9103,#9105,#9106))
REPRESENTATION_CONTEXT('','3D')
);
#9102=(
GEOMETRIC_REPRESENTATION_CONTEXT(3)
GLOBAL_UNCERTAINTY_ASSIGNED_CONTEXT((#9069))
GLOBAL_UNIT_ASSIGNED_CONTEXT((#9103,#9105,#9106))
REPRESENTATION_CONTEXT('','3D')
);
#9103=(
LENGTH_UNIT()
NAMED_UNIT(*)
SI_UNIT(.CENTI.,.METRE.)
);
#9104=(
LENGTH_UNIT()
NAMED_UNIT(*)
SI_UNIT($,.METRE.)
);
#9105=(
NAMED_UNIT(*)
PLANE_ANGLE_UNIT()
SI_UNIT($,.RADIAN.)
);
#9106=(
NAMED_UNIT(*)
SI_UNIT($,.STERADIAN.)
SOLID_ANGLE_UNIT()
);
#9107=SHAPE_DEFINITION_REPRESENTATION(#9139,#9227);
#9108=SHAPE_DEFINITION_REPRESENTATION(#9140,#9228);
#9109=SHAPE_DEFINITION_REPRESENTATION(#9141,#9229);
#9110=SHAPE_DEFINITION_REPRESENTATION(#9142,#9230);
#9111=SHAPE_DEFINITION_REPRESENTATION(#9143,#9231);
#9112=SHAPE_DEFINITION_REPRESENTATION(#9144,#9232);
#9113=SHAPE_DEFINITION_REPRESENTATION(#9145,#9233);
#9114=SHAPE_DEFINITION_REPRESENTATION(#9146,#9234);
#9115=SHAPE_DEFINITION_REPRESENTATION(#9147,#9235);
#9116=SHAPE_DEFINITION_REPRESENTATION(#9148,#9236);
#9117=SHAPE_DEFINITION_REPRESENTATION(#9149,#9237);
#9118=SHAPE_DEFINITION_REPRESENTATION(#9150,#9238);
#9119=SHAPE_DEFINITION_REPRESENTATION(#9151,#9239);
#9120=SHAPE_DEFINITION_REPRESENTATION(#9152,#9240);
#9121=SHAPE_DEFINITION_REPRESENTATION(#9153,#9241);
#9122=SHAPE_DEFINITION_REPRESENTATION(#9154,#9242);
#9123=SHAPE_DEFINITION_REPRESENTATION(#9157,#9243);
#9124=SHAPE_DEFINITION_REPRESENTATION(#9158,#9244);
#9125=SHAPE_DEFINITION_REPRESENTATION(#9159,#9245);
#9126=SHAPE_DEFINITION_REPRESENTATION(#9160,#9246);
#9127=SHAPE_DEFINITION_REPRESENTATION(#9161,#9247);
#9128=SHAPE_DEFINITION_REPRESENTATION(#9162,#9248);
#9129=SHAPE_DEFINITION_REPRESENTATION(#9204,#9249);
#9130=SHAPE_DEFINITION_REPRESENTATION(#9205,#9250);
#9131=SHAPE_DEFINITION_REPRESENTATION(#9206,#9251);
#9132=SHAPE_DEFINITION_REPRESENTATION(#9207,#9252);
#9133=SHAPE_DEFINITION_REPRESENTATION(#9208,#9253);
#9134=SHAPE_DEFINITION_REPRESENTATION(#9209,#9254);
#9135=SHAPE_DEFINITION_REPRESENTATION(#9210,#9255);
#9136=SHAPE_DEFINITION_REPRESENTATION(#9211,#9256);
#9137=SHAPE_DEFINITION_REPRESENTATION(#9212,#9257);
#9138=SHAPE_DEFINITION_REPRESENTATION(#9213,#9258);
#9139=PRODUCT_DEFINITION_SHAPE('',$,#9260);
#9140=PRODUCT_DEFINITION_SHAPE('',$,#9261);
#9141=PRODUCT_DEFINITION_SHAPE('',$,#9262);
#9142=PRODUCT_DEFINITION_SHAPE('',$,#9263);
#9143=PRODUCT_DEFINITION_SHAPE('',$,#9264);
#9144=PRODUCT_DEFINITION_SHAPE('',$,#9265);
#9145=PRODUCT_DEFINITION_SHAPE('',$,#9266);
#9146=PRODUCT_DEFINITION_SHAPE('',$,#9267);
#9147=PRODUCT_DEFINITION_SHAPE('',$,#9268);
#9148=PRODUCT_DEFINITION_SHAPE('',$,#9269);
#9149=PRODUCT_DEFINITION_SHAPE('',$,#9270);
#9150=PRODUCT_DEFINITION_SHAPE('',$,#9271);
#9151=PRODUCT_DEFINITION_SHAPE('',$,#9272);
#9152=PRODUCT_DEFINITION_SHAPE('',$,#9273);
#9153=PRODUCT_DEFINITION_SHAPE('',$,#9274);
#9154=PRODUCT_DEFINITION_SHAPE('',$,#9275);
#9155=PRODUCT_DEFINITION_SHAPE($,$,#203);
#9156=PRODUCT_DEFINITION_SHAPE($,$,#204);
#9157=PRODUCT_DEFINITION_SHAPE('',$,#9276);
#9158=PRODUCT_DEFINITION_SHAPE('',$,#9277);
#9159=PRODUCT_DEFINITION_SHAPE('',$,#9278);
#9160=PRODUCT_DEFINITION_SHAPE('',$,#9279);
#9161=PRODUCT_DEFINITION_SHAPE('',$,#9280);
#9162=PRODUCT_DEFINITION_SHAPE('',$,#9281);
#9163=PRODUCT_DEFINITION_SHAPE($,$,#205);
#9164=PRODUCT_DEFINITION_SHAPE($,$,#206);
#9165=PRODUCT_DEFINITION_SHAPE($,$,#207);
#9166=PRODUCT_DEFINITION_SHAPE($,$,#208);
#9167=PRODUCT_DEFINITION_SHAPE($,$,#209);
#9168=PRODUCT_DEFINITION_SHAPE($,$,#210);
#9169=PRODUCT_DEFINITION_SHAPE($,$,#211);
#9170=PRODUCT_DEFINITION_SHAPE($,$,#212);
#9171=PRODUCT_DEFINITION_SHAPE($,$,#213);
#9172=PRODUCT_DEFINITION_SHAPE($,$,#214);
#9173=PRODUCT_DEFINITION_SHAPE($,$,#215);
#9174=PRODUCT_DEFINITION_SHAPE($,$,#216);
#9175=PRODUCT_DEFINITION_SHAPE($,$,#217);
#9176=PRODUCT_DEFINITION_SHAPE($,$,#218);
#9177=PRODUCT_DEFINITION_SHAPE($,$,#219);
#9178=PRODUCT_DEFINITION_SHAPE($,$,#220);
#9179=PRODUCT_DEFINITION_SHAPE($,$,#221);
#9180=PRODUCT_DEFINITION_SHAPE($,$,#222);
#9181=PRODUCT_DEFINITION_SHAPE($,$,#223);
#9182=PRODUCT_DEFINITION_SHAPE($,$,#224);
#9183=PRODUCT_DEFINITION_SHAPE($,$,#225);
#9184=PRODUCT_DEFINITION_SHAPE($,$,#226);
#9185=PRODUCT_DEFINITION_SHAPE($,$,#227);
#9186=PRODUCT_DEFINITION_SHAPE($,$,#228);
#9187=PRODUCT_DEFINITION_SHAPE($,$,#229);
#9188=PRODUCT_DEFINITION_SHAPE($,$,#230);
#9189=PRODUCT_DEFINITION_SHAPE($,$,#231);
#9190=PRODUCT_DEFINITION_SHAPE($,$,#232);
#9191=PRODUCT_DEFINITION_SHAPE($,$,#233);
#9192=PRODUCT_DEFINITION_SHAPE($,$,#234);
#9193=PRODUCT_DEFINITION_SHAPE($,$,#235);
#9194=PRODUCT_DEFINITION_SHAPE($,$,#236);
#9195=PRODUCT_DEFINITION_SHAPE($,$,#237);
#9196=PRODUCT_DEFINITION_SHAPE($,$,#238);
#9197=PRODUCT_DEFINITION_SHAPE($,$,#239);
#9198=PRODUCT_DEFINITION_SHAPE($,$,#240);
#9199=PRODUCT_DEFINITION_SHAPE($,$,#241);
#9200=PRODUCT_DEFINITION_SHAPE($,$,#242);
#9201=PRODUCT_DEFINITION_SHAPE($,$,#243);
#9202=PRODUCT_DEFINITION_SHAPE($,$,#244);
#9203=PRODUCT_DEFINITION_SHAPE($,$,#245);
#9204=PRODUCT_DEFINITION_SHAPE('',$,#9282);
#9205=PRODUCT_DEFINITION_SHAPE('',$,#9283);
#9206=PRODUCT_DEFINITION_SHAPE('',$,#9284);
#9207=PRODUCT_DEFINITION_SHAPE('',$,#9285);
#9208=PRODUCT_DEFINITION_SHAPE('',$,#9286);
#9209=PRODUCT_DEFINITION_SHAPE('',$,#9287);
#9210=PRODUCT_DEFINITION_SHAPE('',$,#9288);
#9211=PRODUCT_DEFINITION_SHAPE('',$,#9289);
#9212=PRODUCT_DEFINITION_SHAPE('',$,#9290);
#9213=PRODUCT_DEFINITION_SHAPE('',$,#9291);
#9214=PRODUCT_DEFINITION_SHAPE($,$,#246);
#9215=PRODUCT_DEFINITION_SHAPE($,$,#247);
#9216=PRODUCT_DEFINITION_SHAPE($,$,#248);
#9217=PRODUCT_DEFINITION_SHAPE($,$,#249);
#9218=PRODUCT_DEFINITION_SHAPE($,$,#250);
#9219=PRODUCT_DEFINITION_SHAPE($,$,#251);
#9220=PRODUCT_DEFINITION_SHAPE($,$,#252);
#9221=PRODUCT_DEFINITION_SHAPE($,$,#253);
#9222=PRODUCT_DEFINITION_SHAPE($,$,#254);
#9223=PRODUCT_DEFINITION_SHAPE($,$,#255);
#9224=PRODUCT_DEFINITION_SHAPE($,$,#256);
#9225=PRODUCT_DEFINITION_SHAPE($,$,#257);
#9226=PRODUCT_DEFINITION_SHAPE($,$,#258);
#9227=SHAPE_REPRESENTATION('',(#5263,#5889,#5890),#9070);
#9228=SHAPE_REPRESENTATION('',(#5264,#5696,#5697,#5698,#5699,#5700,#5701,
#5702,#5703,#5704,#5705,#5706,#5707,#5708,#5709,#5710,#5711,#5712,#5713,
#5714,#5715,#5716,#5717,#5718,#5719,#5720,#5721,#5722,#5723,#5724,#5725,
#5726,#5727,#5728,#5729,#5730,#5731,#5732,#5733,#5734,#5735,#5736),#9071);
#9229=SHAPE_REPRESENTATION('',(#5265),#9072);
#9230=SHAPE_REPRESENTATION('',(#5335),#9073);
#9231=SHAPE_REPRESENTATION('',(#5379),#9074);
#9232=SHAPE_REPRESENTATION('',(#5391),#9075);
#9233=SHAPE_REPRESENTATION('',(#5458),#9076);
#9234=SHAPE_REPRESENTATION('',(#5502),#9077);
#9235=SHAPE_REPRESENTATION('',(#5514),#9078);
#9236=SHAPE_REPRESENTATION('',(#5523),#9079);
#9237=SHAPE_REPRESENTATION('',(#5532),#9080);
#9238=SHAPE_REPRESENTATION('',(#5541),#9081);
#9239=SHAPE_REPRESENTATION('',(#5568),#9082);
#9240=SHAPE_REPRESENTATION('',(#5594,#5636,#5637),#9083);
#9241=SHAPE_REPRESENTATION('',(#5595),#9084);
#9242=SHAPE_REPRESENTATION('',(#5623),#9085);
#9243=SHAPE_REPRESENTATION('',(#5638),#9086);
#9244=SHAPE_REPRESENTATION('',(#5642),#9087);
#9245=SHAPE_REPRESENTATION('',(#5659),#9088);
#9246=SHAPE_REPRESENTATION('',(#5663),#9089);
#9247=SHAPE_REPRESENTATION('',(#5669),#9090);
#9248=SHAPE_REPRESENTATION('',(#5680),#9091);
#9249=SHAPE_REPRESENTATION('',(#5737,#5878,#5879,#5880,#5881,#5882,#5883,
#5884,#5885,#5886,#5887,#5888),#9092);
#9250=SHAPE_REPRESENTATION('',(#5738),#9093);
#9251=SHAPE_REPRESENTATION('',(#5759),#9094);
#9252=SHAPE_REPRESENTATION('',(#5763),#9095);
#9253=SHAPE_REPRESENTATION('',(#5773),#9096);
#9254=SHAPE_REPRESENTATION('',(#5799),#9097);
#9255=SHAPE_REPRESENTATION('',(#5826),#9098);
#9256=SHAPE_REPRESENTATION('',(#5843),#9099);
#9257=SHAPE_REPRESENTATION('',(#5858),#9100);
#9258=SHAPE_REPRESENTATION('',(#5867),#9101);
#9259=PRODUCT_DEFINITION_CONTEXT('part definition',#9357,'design');
#9260=PRODUCT_DEFINITION('PAT-028',
'PAT-028',#9292,#9259);
#9261=PRODUCT_DEFINITION(
'Twenty millimetre bore cylinder and flow controls',
'Twenty millimetre bore cylinder and flow controls',#9293,#9259);
#9262=PRODUCT_DEFINITION('Front cylinder cap','Front cylinder cap',#9294,
#9259);
#9263=PRODUCT_DEFINITION('Needle flow-control fitting',
'Needle flow-control fitting',#9295,#9259);
#9264=PRODUCT_DEFINITION('Metering needle and grip',
'Metering needle and grip',#9296,#9259);
#9265=PRODUCT_DEFINITION('Rear cylinder cap','Rear cylinder cap',#9297,
#9259);
#9266=PRODUCT_DEFINITION('Needle flow-control fitting (1)',
'Needle flow-control fitting (1)',#9298,#9259);
#9267=PRODUCT_DEFINITION('Metering needle and grip (1)',
'Metering needle and grip (1)',#9299,#9259);
#9268=PRODUCT_DEFINITION('Twenty millimetre bore barrel',
'Twenty millimetre bore barrel',#9300,#9259);
#9269=PRODUCT_DEFINITION('Barrel end gasket','Barrel end gasket',#9301,
#9259);
#9270=PRODUCT_DEFINITION('Barrel end gasket (1)','Barrel end gasket (1)',
#9302,#9259);
#9271=PRODUCT_DEFINITION('Mounting foot','Mounting foot',#9303,#9259);
#9272=PRODUCT_DEFINITION('Cap Screw - M5x20','Cap Screw - M5x20',#9304,
#9259);
#9273=PRODUCT_DEFINITION(
'Push-In Tube Fitting - 6 mm Tube, 1-8 Inch Tapered Pipe Thread',
'Push-In Tube Fitting - 6 mm Tube, 1-8 Inch Tapered Pipe Thread',#9305,
#9259);
#9274=PRODUCT_DEFINITION('Body','Body',#9306,#9259);
#9275=PRODUCT_DEFINITION('Release collar','Release collar',#9307,#9259);
#9276=PRODUCT_DEFINITION('O-Ring','O-Ring',#9308,#9259);
#9277=PRODUCT_DEFINITION('Rod guide','Rod guide',#9309,#9259);
#9278=PRODUCT_DEFINITION('Rod seal','Rod seal',#9310,#9259);
#9279=PRODUCT_DEFINITION('M5 tie rod','M5 tie rod',#9311,#9259);
#9280=PRODUCT_DEFINITION('Flat Washer - M5','Flat Washer - M5',#9312,#9259);
#9281=PRODUCT_DEFINITION('Hex Nut - M5','Hex Nut - M5',#9313,#9259);
#9282=PRODUCT_DEFINITION('Piston rod and clevis',
'Piston rod and clevis',#9314,#9259);
#9283=PRODUCT_DEFINITION('Twenty millimetre piston',
'Twenty millimetre piston',#9315,#9259);
#9284=PRODUCT_DEFINITION('Piston seal','Piston seal',#9316,#9259);
#9285=PRODUCT_DEFINITION('Piston rod','Piston rod',#9317,#9259);
#9286=PRODUCT_DEFINITION('Cap Screw - M4x16','Cap Screw - M4x16',#9318,
#9259);
#9287=PRODUCT_DEFINITION('Six-millimetre-pin rod clevis',
'Six-millimetre-pin rod clevis',#9319,#9259);
#9288=PRODUCT_DEFINITION('Socket Set Screw - M4x6',
'Socket Set Screw - M4x6',#9320,#9259);
#9289=PRODUCT_DEFINITION('Clevis Pin - 6x30','Clevis Pin - 6x30',#9321,
#9259);
#9290=PRODUCT_DEFINITION('Flat Washer - M6','Flat Washer - M6',#9322,#9259);
#9291=PRODUCT_DEFINITION('Split Pin - 1.6x16','Split Pin - 1.6x16',#9323,
#9259);
#9292=PRODUCT_DEFINITION_FORMATION('',$,#9359);
#9293=PRODUCT_DEFINITION_FORMATION('',$,#9360);
#9294=PRODUCT_DEFINITION_FORMATION('',$,#9361);
#9295=PRODUCT_DEFINITION_FORMATION('',$,#9362);
#9296=PRODUCT_DEFINITION_FORMATION('',$,#9363);
#9297=PRODUCT_DEFINITION_FORMATION('',$,#9364);
#9298=PRODUCT_DEFINITION_FORMATION('',$,#9365);
#9299=PRODUCT_DEFINITION_FORMATION('',$,#9366);
#9300=PRODUCT_DEFINITION_FORMATION('',$,#9367);
#9301=PRODUCT_DEFINITION_FORMATION('',$,#9368);
#9302=PRODUCT_DEFINITION_FORMATION('',$,#9369);
#9303=PRODUCT_DEFINITION_FORMATION('',$,#9370);
#9304=PRODUCT_DEFINITION_FORMATION('',$,#9371);
#9305=PRODUCT_DEFINITION_FORMATION('',$,#9372);
#9306=PRODUCT_DEFINITION_FORMATION('',$,#9373);
#9307=PRODUCT_DEFINITION_FORMATION('',$,#9374);
#9308=PRODUCT_DEFINITION_FORMATION('',$,#9375);
#9309=PRODUCT_DEFINITION_FORMATION('',$,#9376);
#9310=PRODUCT_DEFINITION_FORMATION('',$,#9377);
#9311=PRODUCT_DEFINITION_FORMATION('',$,#9378);
#9312=PRODUCT_DEFINITION_FORMATION('',$,#9379);
#9313=PRODUCT_DEFINITION_FORMATION('',$,#9380);
#9314=PRODUCT_DEFINITION_FORMATION('',$,#9381);
#9315=PRODUCT_DEFINITION_FORMATION('',$,#9382);
#9316=PRODUCT_DEFINITION_FORMATION('',$,#9383);
#9317=PRODUCT_DEFINITION_FORMATION('',$,#9384);
#9318=PRODUCT_DEFINITION_FORMATION('',$,#9385);
#9319=PRODUCT_DEFINITION_FORMATION('',$,#9386);
#9320=PRODUCT_DEFINITION_FORMATION('',$,#9387);
#9321=PRODUCT_DEFINITION_FORMATION('',$,#9388);
#9322=PRODUCT_DEFINITION_FORMATION('',$,#9389);
#9323=PRODUCT_DEFINITION_FORMATION('',$,#9390);
#9324=PRODUCT_RELATED_PRODUCT_CATEGORY('PAT-028','PAT-028',(#9359));
#9325=PRODUCT_RELATED_PRODUCT_CATEGORY(
'Twenty millimetre bore cylinder and flow controls',
'Twenty millimetre bore cylinder and flow controls',(#9360));
#9326=PRODUCT_RELATED_PRODUCT_CATEGORY('Front cylinder cap',
'Front cylinder cap',(#9361));
#9327=PRODUCT_RELATED_PRODUCT_CATEGORY('Needle flow-control fitting',
'Needle flow-control fitting',(#9362));
#9328=PRODUCT_RELATED_PRODUCT_CATEGORY('Metering needle and grip',
'Metering needle and grip',(#9363));
#9329=PRODUCT_RELATED_PRODUCT_CATEGORY('Rear cylinder cap',
'Rear cylinder cap',(#9364));
#9330=PRODUCT_RELATED_PRODUCT_CATEGORY(
'Needle flow-control fitting (1)','Needle flow-control fitting (1)',(#9365));
#9331=PRODUCT_RELATED_PRODUCT_CATEGORY('Metering needle and grip (1)',
'Metering needle and grip (1)',(#9366));
#9332=PRODUCT_RELATED_PRODUCT_CATEGORY('Twenty millimetre bore barrel',
'Twenty millimetre bore barrel',(#9367));
#9333=PRODUCT_RELATED_PRODUCT_CATEGORY('Barrel end gasket',
'Barrel end gasket',(#9368));
#9334=PRODUCT_RELATED_PRODUCT_CATEGORY('Barrel end gasket (1)',
'Barrel end gasket (1)',(#9369));
#9335=PRODUCT_RELATED_PRODUCT_CATEGORY('Mounting foot','Mounting foot',
(#9370));
#9336=PRODUCT_RELATED_PRODUCT_CATEGORY('Cap Screw - M5x20',
'Cap Screw - M5x20',(#9371));
#9337=PRODUCT_RELATED_PRODUCT_CATEGORY(
'Push-In Tube Fitting - 6 mm Tube, 1-8 Inch Tapered Pipe Thread',
'Push-In Tube Fitting - 6 mm Tube, 1-8 Inch Tapered Pipe Thread',(#9372));
#9338=PRODUCT_RELATED_PRODUCT_CATEGORY('Body','Body',(#9373));
#9339=PRODUCT_RELATED_PRODUCT_CATEGORY('Release collar',
'Release collar',(#9374));
#9340=PRODUCT_RELATED_PRODUCT_CATEGORY('O-Ring','O-Ring',(#9375));
#9341=PRODUCT_RELATED_PRODUCT_CATEGORY('Rod guide','Rod guide',(#9376));
#9342=PRODUCT_RELATED_PRODUCT_CATEGORY('Rod seal','Rod seal',(#9377));
#9343=PRODUCT_RELATED_PRODUCT_CATEGORY('M5 tie rod','M5 tie rod',(#9378));
#9344=PRODUCT_RELATED_PRODUCT_CATEGORY('Flat Washer - M5',
'Flat Washer - M5',(#9379));
#9345=PRODUCT_RELATED_PRODUCT_CATEGORY('Hex Nut - M5','Hex Nut - M5',(#9380));
#9346=PRODUCT_RELATED_PRODUCT_CATEGORY('Piston rod and clevis',
'Piston rod and clevis',(#9381));
#9347=PRODUCT_RELATED_PRODUCT_CATEGORY('Twenty millimetre piston',
'Twenty millimetre piston',(#9382));
#9348=PRODUCT_RELATED_PRODUCT_CATEGORY('Piston seal','Piston seal',(#9383));
#9349=PRODUCT_RELATED_PRODUCT_CATEGORY('Piston rod','Piston rod',(#9384));
#9350=PRODUCT_RELATED_PRODUCT_CATEGORY('Cap Screw - M4x16',
'Cap Screw - M4x16',(#9385));
#9351=PRODUCT_RELATED_PRODUCT_CATEGORY('Six-millimetre-pin rod clevis',
'Six-millimetre-pin rod clevis',(#9386));
#9352=PRODUCT_RELATED_PRODUCT_CATEGORY('Socket Set Screw - M4x6',
'Socket Set Screw - M4x6',(#9387));
#9353=PRODUCT_RELATED_PRODUCT_CATEGORY('Clevis Pin - 6x30',
'Clevis Pin - 6x30',(#9388));
#9354=PRODUCT_RELATED_PRODUCT_CATEGORY('Flat Washer - M6',
'Flat Washer - M6',(#9389));
#9355=PRODUCT_RELATED_PRODUCT_CATEGORY('Split Pin - 1.6x16',
'Split Pin - 1.6x16',(#9390));
#9356=APPLICATION_PROTOCOL_DEFINITION('international standard',
'automotive_design',2009,#9357);
#9357=APPLICATION_CONTEXT(
'Core Data for Automotive Mechanical Design Process');
#9358=PRODUCT_CONTEXT('part definition',#9357,'mechanical');
#9359=PRODUCT('PAT-028','PAT-028',
'PAT-028',(#9358));
#9360=PRODUCT('Twenty millimetre bore cylinder and flow controls',
'Twenty millimetre bore cylinder and flow controls',
'Twenty millimetre bore cylinder and flow controls',(#9358));
#9361=PRODUCT('Front cylinder cap','Front cylinder cap',
'Front cylinder cap',(#9358));
#9362=PRODUCT('Needle flow-control fitting',
'Needle flow-control fitting','Needle flow-control fitting',(#9358));
#9363=PRODUCT('Metering needle and grip','Metering needle and grip',
'Metering needle and grip',(#9358));
#9364=PRODUCT('Rear cylinder cap','Rear cylinder cap',
'Rear cylinder cap',(#9358));
#9365=PRODUCT('Needle flow-control fitting (1)',
'Needle flow-control fitting (1)','Needle flow-control fitting (1)',(#9358));
#9366=PRODUCT('Metering needle and grip (1)',
'Metering needle and grip (1)','Metering needle and grip (1)',(#9358));
#9367=PRODUCT('Twenty millimetre bore barrel',
'Twenty millimetre bore barrel','Twenty millimetre bore barrel',(#9358));
#9368=PRODUCT('Barrel end gasket','Barrel end gasket',
'Barrel end gasket',(#9358));
#9369=PRODUCT('Barrel end gasket (1)','Barrel end gasket (1)',
'Barrel end gasket (1)',(#9358));
#9370=PRODUCT('Mounting foot','Mounting foot','Mounting foot',(#9358));
#9371=PRODUCT('Cap Screw - M5x20','Cap Screw - M5x20',
'Cap Screw - M5x20',(#9358));
#9372=PRODUCT(
'Push-In Tube Fitting - 6 mm Tube, 1-8 Inch Tapered Pipe Thread',
'Push-In Tube Fitting - 6 mm Tube, 1-8 Inch Tapered Pipe Thread',
'Push-In Tube Fitting - 6 mm Tube, 1-8 Inch Tapered Pipe Thread',(#9358));
#9373=PRODUCT('Body','Body','Body',(#9358));
#9374=PRODUCT('Release collar','Release collar','Release collar',(#9358));
#9375=PRODUCT('O-Ring','O-Ring','O-Ring',(#9358));
#9376=PRODUCT('Rod guide','Rod guide','Rod guide',(#9358));
#9377=PRODUCT('Rod seal','Rod seal','Rod seal',(#9358));
#9378=PRODUCT('M5 tie rod','M5 tie rod','M5 tie rod',(#9358));
#9379=PRODUCT('Flat Washer - M5','Flat Washer - M5','Flat Washer - M5',
(#9358));
#9380=PRODUCT('Hex Nut - M5','Hex Nut - M5','Hex Nut - M5',(#9358));
#9381=PRODUCT('Piston rod and clevis','Piston rod and clevis',
'Piston rod and clevis',(#9358));
#9382=PRODUCT('Twenty millimetre piston','Twenty millimetre piston',
'Twenty millimetre piston',(#9358));
#9383=PRODUCT('Piston seal','Piston seal','Piston seal',(#9358));
#9384=PRODUCT('Piston rod','Piston rod','Piston rod',(#9358));
#9385=PRODUCT('Cap Screw - M4x16','Cap Screw - M4x16',
'Cap Screw - M4x16',(#9358));
#9386=PRODUCT('Six-millimetre-pin rod clevis',
'Six-millimetre-pin rod clevis','Six-millimetre-pin rod clevis',(#9358));
#9387=PRODUCT('Socket Set Screw - M4x6','Socket Set Screw - M4x6',
'Socket Set Screw - M4x6',(#9358));
#9388=PRODUCT('Clevis Pin - 6x30','Clevis Pin - 6x30',
'Clevis Pin - 6x30',(#9358));
#9389=PRODUCT('Flat Washer - M6','Flat Washer - M6','Flat Washer - M6',
(#9358));
#9390=PRODUCT('Split Pin - 1.6x16','Split Pin - 1.6x16',
'Split Pin - 1.6x16',(#9358));
#9391=PRESENTATION_STYLE_ASSIGNMENT((#9397));
#9392=PRESENTATION_STYLE_ASSIGNMENT((#9398));
#9393=PRESENTATION_STYLE_ASSIGNMENT((#9399));
#9394=PRESENTATION_STYLE_ASSIGNMENT((#9400));
#9395=PRESENTATION_STYLE_ASSIGNMENT((#9401));
#9396=PRESENTATION_STYLE_ASSIGNMENT((#9402));
#9397=SURFACE_STYLE_USAGE(.BOTH.,#9403);
#9398=SURFACE_STYLE_USAGE(.BOTH.,#9404);
#9399=SURFACE_STYLE_USAGE(.BOTH.,#9405);
#9400=SURFACE_STYLE_USAGE(.BOTH.,#9406);
#9401=SURFACE_STYLE_USAGE(.BOTH.,#9407);
#9402=SURFACE_STYLE_USAGE(.BOTH.,#9408);
#9403=SURFACE_SIDE_STYLE('',(#9409));
#9404=SURFACE_SIDE_STYLE('',(#9410));
#9405=SURFACE_SIDE_STYLE('',(#9411));
#9406=SURFACE_SIDE_STYLE('',(#9412));
#9407=SURFACE_SIDE_STYLE('',(#9413));
#9408=SURFACE_SIDE_STYLE('',(#9414));
#9409=SURFACE_STYLE_FILL_AREA(#9415);
#9410=SURFACE_STYLE_FILL_AREA(#9416);
#9411=SURFACE_STYLE_FILL_AREA(#9417);
#9412=SURFACE_STYLE_FILL_AREA(#9418);
#9413=SURFACE_STYLE_FILL_AREA(#9419);
#9414=SURFACE_STYLE_FILL_AREA(#9420);
#9415=FILL_AREA_STYLE('Steel - Satin',(#9421));
#9416=FILL_AREA_STYLE('CAD Library Painted - Engineering blue',(#9422));
#9417=FILL_AREA_STYLE('CAD Library Painted - Graphite',(#9423));
#9418=FILL_AREA_STYLE('CAD Library Painted - Off white',(#9424));
#9419=FILL_AREA_STYLE('CAD Library Painted - Deep blue',(#9425));
#9420=FILL_AREA_STYLE('CAD Library Painted - Steel gray',(#9426));
#9421=FILL_AREA_STYLE_COLOUR('Steel - Satin',#9427);
#9422=FILL_AREA_STYLE_COLOUR('CAD Library Painted - Engineering blue',#9428);
#9423=FILL_AREA_STYLE_COLOUR('CAD Library Painted - Graphite',#9429);
#9424=FILL_AREA_STYLE_COLOUR('CAD Library Painted - Off white',#9430);
#9425=FILL_AREA_STYLE_COLOUR('CAD Library Painted - Deep blue',#9431);
#9426=FILL_AREA_STYLE_COLOUR('CAD Library Painted - Steel gray',#9432);
#9427=COLOUR_RGB('Steel - Satin',0.627450980392157,0.627450980392157,0.627450980392157);
#9428=COLOUR_RGB('CAD Library Painted - Engineering blue',0.12156862745098,
0.356862745098039,0.6);
#9429=COLOUR_RGB('CAD Library Painted - Graphite',0.0980392156862745,0.109803921568627,
0.125490196078431);
#9430=COLOUR_RGB('CAD Library Painted - Off white',0.909803921568627,0.901960784313726,
0.858823529411765);
#9431=COLOUR_RGB('CAD Library Painted - Deep blue',0.0784313725490196,0.203921568627451,
0.349019607843137);
#9432=COLOUR_RGB('CAD Library Painted - Steel gray',0.592156862745098,0.631372549019608,
0.67843137254902);
#9433=COLOUR_RGB('Dark Blue',0.08,0.2,0.34);
#9434=FILL_AREA_STYLE_COLOUR('',#9433);
#9435=FILL_AREA_STYLE('',(#9434));
#9436=SURFACE_STYLE_FILL_AREA(#9435);
#9437=SURFACE_SIDE_STYLE('',(#9436));
#9438=SURFACE_STYLE_USAGE(.BOTH.,#9437);
#9439=PRESENTATION_STYLE_ASSIGNMENT((#9438));
#9440=COLOUR_RGB('Light Blue',0.38,0.62,0.78);
#9441=FILL_AREA_STYLE_COLOUR('',#9440);
#9442=FILL_AREA_STYLE('',(#9441));
#9443=SURFACE_STYLE_FILL_AREA(#9442);
#9444=SURFACE_SIDE_STYLE('',(#9443));
#9445=SURFACE_STYLE_USAGE(.BOTH.,#9444);
#9446=PRESENTATION_STYLE_ASSIGNMENT((#9445));
#9447=COLOUR_RGB('Sky Blue',0.24,0.69,0.87);
#9448=FILL_AREA_STYLE_COLOUR('',#9447);
#9449=FILL_AREA_STYLE('',(#9448));
#9450=SURFACE_STYLE_FILL_AREA(#9449);
#9451=SURFACE_SIDE_STYLE('',(#9450));
#9452=SURFACE_STYLE_USAGE(.BOTH.,#9451);
#9453=PRESENTATION_STYLE_ASSIGNMENT((#9452));
#9454=COLOUR_RGB('Grey',0.48,0.52,0.57);
#9455=FILL_AREA_STYLE_COLOUR('',#9454);
#9456=FILL_AREA_STYLE('',(#9455));
#9457=SURFACE_STYLE_FILL_AREA(#9456);
#9458=SURFACE_SIDE_STYLE('',(#9457));
#9459=SURFACE_STYLE_USAGE(.BOTH.,#9458);
#9460=PRESENTATION_STYLE_ASSIGNMENT((#9459));
#9461=COLOUR_RGB('Black',0.12,0.14,0.17);
#9462=FILL_AREA_STYLE_COLOUR('',#9461);
#9463=FILL_AREA_STYLE('',(#9462));
#9464=SURFACE_STYLE_FILL_AREA(#9463);
#9465=SURFACE_SIDE_STYLE('',(#9464));
#9466=SURFACE_STYLE_USAGE(.BOTH.,#9465);
#9467=PRESENTATION_STYLE_ASSIGNMENT((#9466));
#9468=COLOUR_RGB('Off White',0.89,0.88,0.83);
#9469=FILL_AREA_STYLE_COLOUR('',#9468);
#9470=FILL_AREA_STYLE('',(#9469));
#9471=SURFACE_STYLE_FILL_AREA(#9470);
#9472=SURFACE_SIDE_STYLE('',(#9471));
#9473=SURFACE_STYLE_USAGE(.BOTH.,#9472);
#9474=PRESENTATION_STYLE_ASSIGNMENT((#9473));
ENDSEC;
END-ISO-10303-21;
